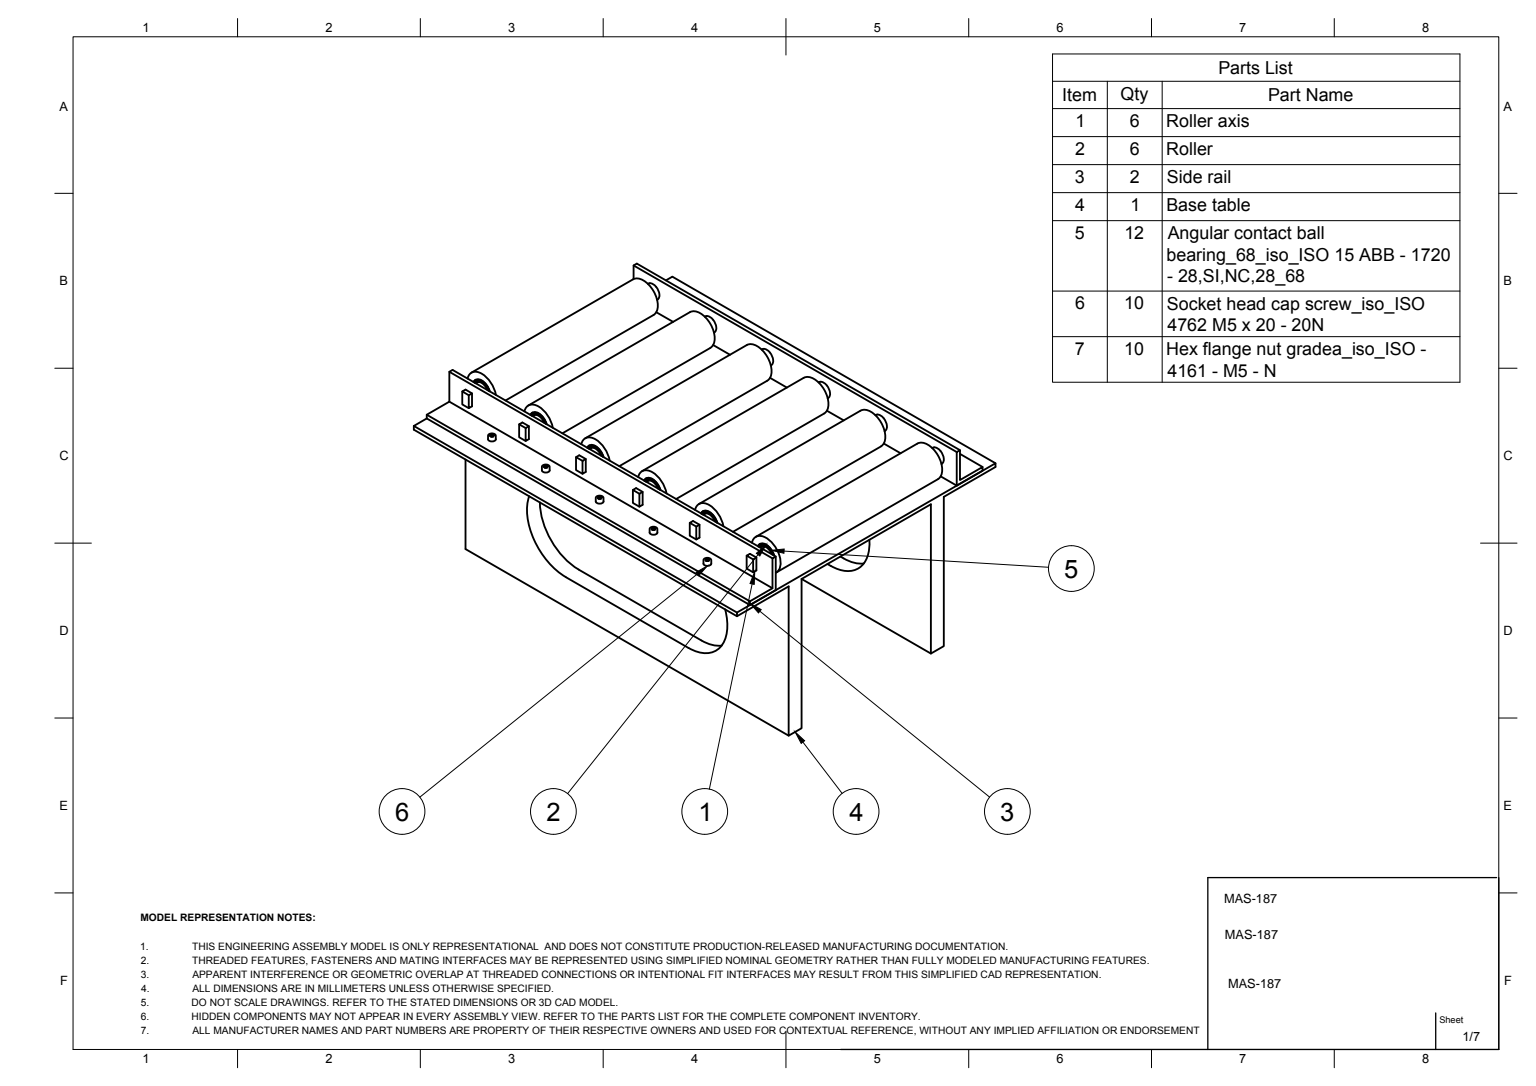
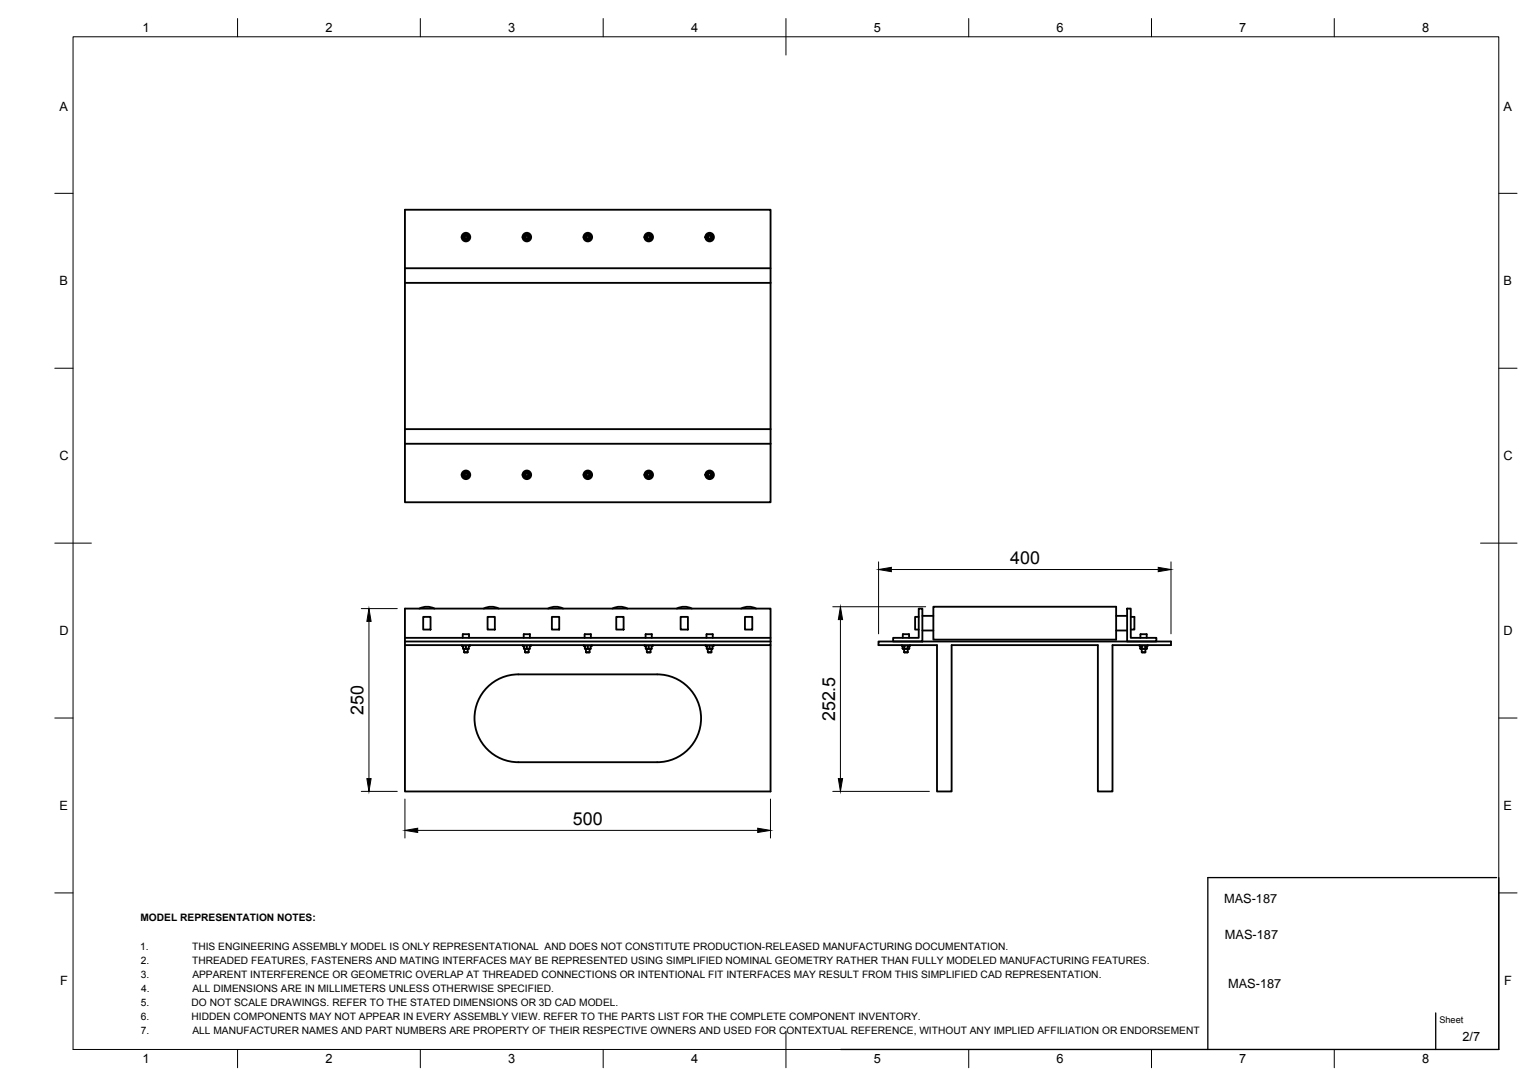
ISO-10303-21;
HEADER;
/* Generated by software containing ST-Developer
 * from STEP Tools, Inc. (www.steptools.com) 
 */

FILE_DESCRIPTION(
/* description */ ('STEP AP214'),
/* implementation_level */ '2;1');

FILE_NAME(
/* name */ 'MAS-187',
/* time_stamp */ '2026-11-04T19:00:26-08:00',
/* author */ (''),
/* organization */ (''),
/* preprocessor_version */ 'ST-DEVELOPER v20.2',
/* originating_system */ 'Autodesk Translation Framework v15.17.0.0',
/* authorisation */ '');

FILE_SCHEMA (('AUTOMOTIVE_DESIGN { 1 0 10303 214 3 1 1 }'));
ENDSEC;

DATA;
#10=MECHANICAL_DESIGN_GEOMETRIC_PRESENTATION_REPRESENTATION('',(#271,#272,
#273,#274,#275,#276,#277),#5689);
#11=ITEM_DEFINED_TRANSFORMATION($,$,#3156,#3322);
#12=ITEM_DEFINED_TRANSFORMATION($,$,#3229,#3323);
#13=ITEM_DEFINED_TRANSFORMATION($,$,#3108,#3324);
#14=ITEM_DEFINED_TRANSFORMATION($,$,#3047,#3325);
#15=ITEM_DEFINED_TRANSFORMATION($,$,#3186,#3326);
#16=ITEM_DEFINED_TRANSFORMATION($,$,#3246,#3327);
#17=ITEM_DEFINED_TRANSFORMATION($,$,#3284,#3328);
#18=ITEM_DEFINED_TRANSFORMATION($,$,#3186,#3329);
#19=ITEM_DEFINED_TRANSFORMATION($,$,#3246,#3330);
#20=ITEM_DEFINED_TRANSFORMATION($,$,#3246,#3331);
#21=ITEM_DEFINED_TRANSFORMATION($,$,#3246,#3332);
#22=ITEM_DEFINED_TRANSFORMATION($,$,#3246,#3333);
#23=ITEM_DEFINED_TRANSFORMATION($,$,#3284,#3334);
#24=ITEM_DEFINED_TRANSFORMATION($,$,#3284,#3335);
#25=ITEM_DEFINED_TRANSFORMATION($,$,#3284,#3336);
#26=ITEM_DEFINED_TRANSFORMATION($,$,#3284,#3337);
#27=ITEM_DEFINED_TRANSFORMATION($,$,#3108,#3338);
#28=ITEM_DEFINED_TRANSFORMATION($,$,#3186,#3339);
#29=ITEM_DEFINED_TRANSFORMATION($,$,#3186,#3340);
#30=ITEM_DEFINED_TRANSFORMATION($,$,#3186,#3341);
#31=ITEM_DEFINED_TRANSFORMATION($,$,#3186,#3342);
#32=ITEM_DEFINED_TRANSFORMATION($,$,#3186,#3343);
#33=ITEM_DEFINED_TRANSFORMATION($,$,#3156,#3344);
#34=ITEM_DEFINED_TRANSFORMATION($,$,#3156,#3345);
#35=ITEM_DEFINED_TRANSFORMATION($,$,#3156,#3346);
#36=ITEM_DEFINED_TRANSFORMATION($,$,#3156,#3347);
#37=ITEM_DEFINED_TRANSFORMATION($,$,#3156,#3348);
#38=ITEM_DEFINED_TRANSFORMATION($,$,#3186,#3349);
#39=ITEM_DEFINED_TRANSFORMATION($,$,#3186,#3350);
#40=ITEM_DEFINED_TRANSFORMATION($,$,#3186,#3351);
#41=ITEM_DEFINED_TRANSFORMATION($,$,#3186,#3352);
#42=ITEM_DEFINED_TRANSFORMATION($,$,#3186,#3353);
#43=ITEM_DEFINED_TRANSFORMATION($,$,#3229,#3354);
#44=ITEM_DEFINED_TRANSFORMATION($,$,#3229,#3355);
#45=ITEM_DEFINED_TRANSFORMATION($,$,#3229,#3356);
#46=ITEM_DEFINED_TRANSFORMATION($,$,#3229,#3357);
#47=ITEM_DEFINED_TRANSFORMATION($,$,#3229,#3358);
#48=ITEM_DEFINED_TRANSFORMATION($,$,#3284,#3359);
#49=ITEM_DEFINED_TRANSFORMATION($,$,#3284,#3360);
#50=ITEM_DEFINED_TRANSFORMATION($,$,#3246,#3361);
#51=ITEM_DEFINED_TRANSFORMATION($,$,#3284,#3362);
#52=ITEM_DEFINED_TRANSFORMATION($,$,#3246,#3363);
#53=ITEM_DEFINED_TRANSFORMATION($,$,#3246,#3364);
#54=ITEM_DEFINED_TRANSFORMATION($,$,#3246,#3365);
#55=ITEM_DEFINED_TRANSFORMATION($,$,#3246,#3366);
#56=ITEM_DEFINED_TRANSFORMATION($,$,#3284,#3367);
#57=ITEM_DEFINED_TRANSFORMATION($,$,#3284,#3368);
#58=(
REPRESENTATION_RELATIONSHIP($,$,#5760,#5757)
REPRESENTATION_RELATIONSHIP_WITH_TRANSFORMATION(#11)
SHAPE_REPRESENTATION_RELATIONSHIP()
);
#59=(
REPRESENTATION_RELATIONSHIP($,$,#5762,#5757)
REPRESENTATION_RELATIONSHIP_WITH_TRANSFORMATION(#12)
SHAPE_REPRESENTATION_RELATIONSHIP()
);
#60=(
REPRESENTATION_RELATIONSHIP($,$,#5759,#5757)
REPRESENTATION_RELATIONSHIP_WITH_TRANSFORMATION(#13)
SHAPE_REPRESENTATION_RELATIONSHIP()
);
#61=(
REPRESENTATION_RELATIONSHIP($,$,#5758,#5757)
REPRESENTATION_RELATIONSHIP_WITH_TRANSFORMATION(#14)
SHAPE_REPRESENTATION_RELATIONSHIP()
);
#62=(
REPRESENTATION_RELATIONSHIP($,$,#5761,#5757)
REPRESENTATION_RELATIONSHIP_WITH_TRANSFORMATION(#15)
SHAPE_REPRESENTATION_RELATIONSHIP()
);
#63=(
REPRESENTATION_RELATIONSHIP($,$,#5763,#5757)
REPRESENTATION_RELATIONSHIP_WITH_TRANSFORMATION(#16)
SHAPE_REPRESENTATION_RELATIONSHIP()
);
#64=(
REPRESENTATION_RELATIONSHIP($,$,#5764,#5757)
REPRESENTATION_RELATIONSHIP_WITH_TRANSFORMATION(#17)
SHAPE_REPRESENTATION_RELATIONSHIP()
);
#65=(
REPRESENTATION_RELATIONSHIP($,$,#5761,#5757)
REPRESENTATION_RELATIONSHIP_WITH_TRANSFORMATION(#18)
SHAPE_REPRESENTATION_RELATIONSHIP()
);
#66=(
REPRESENTATION_RELATIONSHIP($,$,#5763,#5757)
REPRESENTATION_RELATIONSHIP_WITH_TRANSFORMATION(#19)
SHAPE_REPRESENTATION_RELATIONSHIP()
);
#67=(
REPRESENTATION_RELATIONSHIP($,$,#5763,#5757)
REPRESENTATION_RELATIONSHIP_WITH_TRANSFORMATION(#20)
SHAPE_REPRESENTATION_RELATIONSHIP()
);
#68=(
REPRESENTATION_RELATIONSHIP($,$,#5763,#5757)
REPRESENTATION_RELATIONSHIP_WITH_TRANSFORMATION(#21)
SHAPE_REPRESENTATION_RELATIONSHIP()
);
#69=(
REPRESENTATION_RELATIONSHIP($,$,#5763,#5757)
REPRESENTATION_RELATIONSHIP_WITH_TRANSFORMATION(#22)
SHAPE_REPRESENTATION_RELATIONSHIP()
);
#70=(
REPRESENTATION_RELATIONSHIP($,$,#5764,#5757)
REPRESENTATION_RELATIONSHIP_WITH_TRANSFORMATION(#23)
SHAPE_REPRESENTATION_RELATIONSHIP()
);
#71=(
REPRESENTATION_RELATIONSHIP($,$,#5764,#5757)
REPRESENTATION_RELATIONSHIP_WITH_TRANSFORMATION(#24)
SHAPE_REPRESENTATION_RELATIONSHIP()
);
#72=(
REPRESENTATION_RELATIONSHIP($,$,#5764,#5757)
REPRESENTATION_RELATIONSHIP_WITH_TRANSFORMATION(#25)
SHAPE_REPRESENTATION_RELATIONSHIP()
);
#73=(
REPRESENTATION_RELATIONSHIP($,$,#5764,#5757)
REPRESENTATION_RELATIONSHIP_WITH_TRANSFORMATION(#26)
SHAPE_REPRESENTATION_RELATIONSHIP()
);
#74=(
REPRESENTATION_RELATIONSHIP($,$,#5759,#5757)
REPRESENTATION_RELATIONSHIP_WITH_TRANSFORMATION(#27)
SHAPE_REPRESENTATION_RELATIONSHIP()
);
#75=(
REPRESENTATION_RELATIONSHIP($,$,#5761,#5757)
REPRESENTATION_RELATIONSHIP_WITH_TRANSFORMATION(#28)
SHAPE_REPRESENTATION_RELATIONSHIP()
);
#76=(
REPRESENTATION_RELATIONSHIP($,$,#5761,#5757)
REPRESENTATION_RELATIONSHIP_WITH_TRANSFORMATION(#29)
SHAPE_REPRESENTATION_RELATIONSHIP()
);
#77=(
REPRESENTATION_RELATIONSHIP($,$,#5761,#5757)
REPRESENTATION_RELATIONSHIP_WITH_TRANSFORMATION(#30)
SHAPE_REPRESENTATION_RELATIONSHIP()
);
#78=(
REPRESENTATION_RELATIONSHIP($,$,#5761,#5757)
REPRESENTATION_RELATIONSHIP_WITH_TRANSFORMATION(#31)
SHAPE_REPRESENTATION_RELATIONSHIP()
);
#79=(
REPRESENTATION_RELATIONSHIP($,$,#5761,#5757)
REPRESENTATION_RELATIONSHIP_WITH_TRANSFORMATION(#32)
SHAPE_REPRESENTATION_RELATIONSHIP()
);
#80=(
REPRESENTATION_RELATIONSHIP($,$,#5760,#5757)
REPRESENTATION_RELATIONSHIP_WITH_TRANSFORMATION(#33)
SHAPE_REPRESENTATION_RELATIONSHIP()
);
#81=(
REPRESENTATION_RELATIONSHIP($,$,#5760,#5757)
REPRESENTATION_RELATIONSHIP_WITH_TRANSFORMATION(#34)
SHAPE_REPRESENTATION_RELATIONSHIP()
);
#82=(
REPRESENTATION_RELATIONSHIP($,$,#5760,#5757)
REPRESENTATION_RELATIONSHIP_WITH_TRANSFORMATION(#35)
SHAPE_REPRESENTATION_RELATIONSHIP()
);
#83=(
REPRESENTATION_RELATIONSHIP($,$,#5760,#5757)
REPRESENTATION_RELATIONSHIP_WITH_TRANSFORMATION(#36)
SHAPE_REPRESENTATION_RELATIONSHIP()
);
#84=(
REPRESENTATION_RELATIONSHIP($,$,#5760,#5757)
REPRESENTATION_RELATIONSHIP_WITH_TRANSFORMATION(#37)
SHAPE_REPRESENTATION_RELATIONSHIP()
);
#85=(
REPRESENTATION_RELATIONSHIP($,$,#5761,#5757)
REPRESENTATION_RELATIONSHIP_WITH_TRANSFORMATION(#38)
SHAPE_REPRESENTATION_RELATIONSHIP()
);
#86=(
REPRESENTATION_RELATIONSHIP($,$,#5761,#5757)
REPRESENTATION_RELATIONSHIP_WITH_TRANSFORMATION(#39)
SHAPE_REPRESENTATION_RELATIONSHIP()
);
#87=(
REPRESENTATION_RELATIONSHIP($,$,#5761,#5757)
REPRESENTATION_RELATIONSHIP_WITH_TRANSFORMATION(#40)
SHAPE_REPRESENTATION_RELATIONSHIP()
);
#88=(
REPRESENTATION_RELATIONSHIP($,$,#5761,#5757)
REPRESENTATION_RELATIONSHIP_WITH_TRANSFORMATION(#41)
SHAPE_REPRESENTATION_RELATIONSHIP()
);
#89=(
REPRESENTATION_RELATIONSHIP($,$,#5761,#5757)
REPRESENTATION_RELATIONSHIP_WITH_TRANSFORMATION(#42)
SHAPE_REPRESENTATION_RELATIONSHIP()
);
#90=(
REPRESENTATION_RELATIONSHIP($,$,#5762,#5757)
REPRESENTATION_RELATIONSHIP_WITH_TRANSFORMATION(#43)
SHAPE_REPRESENTATION_RELATIONSHIP()
);
#91=(
REPRESENTATION_RELATIONSHIP($,$,#5762,#5757)
REPRESENTATION_RELATIONSHIP_WITH_TRANSFORMATION(#44)
SHAPE_REPRESENTATION_RELATIONSHIP()
);
#92=(
REPRESENTATION_RELATIONSHIP($,$,#5762,#5757)
REPRESENTATION_RELATIONSHIP_WITH_TRANSFORMATION(#45)
SHAPE_REPRESENTATION_RELATIONSHIP()
);
#93=(
REPRESENTATION_RELATIONSHIP($,$,#5762,#5757)
REPRESENTATION_RELATIONSHIP_WITH_TRANSFORMATION(#46)
SHAPE_REPRESENTATION_RELATIONSHIP()
);
#94=(
REPRESENTATION_RELATIONSHIP($,$,#5762,#5757)
REPRESENTATION_RELATIONSHIP_WITH_TRANSFORMATION(#47)
SHAPE_REPRESENTATION_RELATIONSHIP()
);
#95=(
REPRESENTATION_RELATIONSHIP($,$,#5764,#5757)
REPRESENTATION_RELATIONSHIP_WITH_TRANSFORMATION(#48)
SHAPE_REPRESENTATION_RELATIONSHIP()
);
#96=(
REPRESENTATION_RELATIONSHIP($,$,#5764,#5757)
REPRESENTATION_RELATIONSHIP_WITH_TRANSFORMATION(#49)
SHAPE_REPRESENTATION_RELATIONSHIP()
);
#97=(
REPRESENTATION_RELATIONSHIP($,$,#5763,#5757)
REPRESENTATION_RELATIONSHIP_WITH_TRANSFORMATION(#50)
SHAPE_REPRESENTATION_RELATIONSHIP()
);
#98=(
REPRESENTATION_RELATIONSHIP($,$,#5764,#5757)
REPRESENTATION_RELATIONSHIP_WITH_TRANSFORMATION(#51)
SHAPE_REPRESENTATION_RELATIONSHIP()
);
#99=(
REPRESENTATION_RELATIONSHIP($,$,#5763,#5757)
REPRESENTATION_RELATIONSHIP_WITH_TRANSFORMATION(#52)
SHAPE_REPRESENTATION_RELATIONSHIP()
);
#100=(
REPRESENTATION_RELATIONSHIP($,$,#5763,#5757)
REPRESENTATION_RELATIONSHIP_WITH_TRANSFORMATION(#53)
SHAPE_REPRESENTATION_RELATIONSHIP()
);
#101=(
REPRESENTATION_RELATIONSHIP($,$,#5763,#5757)
REPRESENTATION_RELATIONSHIP_WITH_TRANSFORMATION(#54)
SHAPE_REPRESENTATION_RELATIONSHIP()
);
#102=(
REPRESENTATION_RELATIONSHIP($,$,#5763,#5757)
REPRESENTATION_RELATIONSHIP_WITH_TRANSFORMATION(#55)
SHAPE_REPRESENTATION_RELATIONSHIP()
);
#103=(
REPRESENTATION_RELATIONSHIP($,$,#5764,#5757)
REPRESENTATION_RELATIONSHIP_WITH_TRANSFORMATION(#56)
SHAPE_REPRESENTATION_RELATIONSHIP()
);
#104=(
REPRESENTATION_RELATIONSHIP($,$,#5764,#5757)
REPRESENTATION_RELATIONSHIP_WITH_TRANSFORMATION(#57)
SHAPE_REPRESENTATION_RELATIONSHIP()
);
#105=CONTEXT_DEPENDENT_SHAPE_REPRESENTATION(#58,#5710);
#106=CONTEXT_DEPENDENT_SHAPE_REPRESENTATION(#59,#5711);
#107=CONTEXT_DEPENDENT_SHAPE_REPRESENTATION(#60,#5712);
#108=CONTEXT_DEPENDENT_SHAPE_REPRESENTATION(#61,#5713);
#109=CONTEXT_DEPENDENT_SHAPE_REPRESENTATION(#62,#5714);
#110=CONTEXT_DEPENDENT_SHAPE_REPRESENTATION(#63,#5715);
#111=CONTEXT_DEPENDENT_SHAPE_REPRESENTATION(#64,#5716);
#112=CONTEXT_DEPENDENT_SHAPE_REPRESENTATION(#65,#5717);
#113=CONTEXT_DEPENDENT_SHAPE_REPRESENTATION(#66,#5718);
#114=CONTEXT_DEPENDENT_SHAPE_REPRESENTATION(#67,#5719);
#115=CONTEXT_DEPENDENT_SHAPE_REPRESENTATION(#68,#5720);
#116=CONTEXT_DEPENDENT_SHAPE_REPRESENTATION(#69,#5721);
#117=CONTEXT_DEPENDENT_SHAPE_REPRESENTATION(#70,#5722);
#118=CONTEXT_DEPENDENT_SHAPE_REPRESENTATION(#71,#5723);
#119=CONTEXT_DEPENDENT_SHAPE_REPRESENTATION(#72,#5724);
#120=CONTEXT_DEPENDENT_SHAPE_REPRESENTATION(#73,#5725);
#121=CONTEXT_DEPENDENT_SHAPE_REPRESENTATION(#74,#5726);
#122=CONTEXT_DEPENDENT_SHAPE_REPRESENTATION(#75,#5727);
#123=CONTEXT_DEPENDENT_SHAPE_REPRESENTATION(#76,#5728);
#124=CONTEXT_DEPENDENT_SHAPE_REPRESENTATION(#77,#5729);
#125=CONTEXT_DEPENDENT_SHAPE_REPRESENTATION(#78,#5730);
#126=CONTEXT_DEPENDENT_SHAPE_REPRESENTATION(#79,#5731);
#127=CONTEXT_DEPENDENT_SHAPE_REPRESENTATION(#80,#5732);
#128=CONTEXT_DEPENDENT_SHAPE_REPRESENTATION(#81,#5733);
#129=CONTEXT_DEPENDENT_SHAPE_REPRESENTATION(#82,#5734);
#130=CONTEXT_DEPENDENT_SHAPE_REPRESENTATION(#83,#5735);
#131=CONTEXT_DEPENDENT_SHAPE_REPRESENTATION(#84,#5736);
#132=CONTEXT_DEPENDENT_SHAPE_REPRESENTATION(#85,#5737);
#133=CONTEXT_DEPENDENT_SHAPE_REPRESENTATION(#86,#5738);
#134=CONTEXT_DEPENDENT_SHAPE_REPRESENTATION(#87,#5739);
#135=CONTEXT_DEPENDENT_SHAPE_REPRESENTATION(#88,#5740);
#136=CONTEXT_DEPENDENT_SHAPE_REPRESENTATION(#89,#5741);
#137=CONTEXT_DEPENDENT_SHAPE_REPRESENTATION(#90,#5742);
#138=CONTEXT_DEPENDENT_SHAPE_REPRESENTATION(#91,#5743);
#139=CONTEXT_DEPENDENT_SHAPE_REPRESENTATION(#92,#5744);
#140=CONTEXT_DEPENDENT_SHAPE_REPRESENTATION(#93,#5745);
#141=CONTEXT_DEPENDENT_SHAPE_REPRESENTATION(#94,#5746);
#142=CONTEXT_DEPENDENT_SHAPE_REPRESENTATION(#95,#5747);
#143=CONTEXT_DEPENDENT_SHAPE_REPRESENTATION(#96,#5748);
#144=CONTEXT_DEPENDENT_SHAPE_REPRESENTATION(#97,#5749);
#145=CONTEXT_DEPENDENT_SHAPE_REPRESENTATION(#98,#5750);
#146=CONTEXT_DEPENDENT_SHAPE_REPRESENTATION(#99,#5751);
#147=CONTEXT_DEPENDENT_SHAPE_REPRESENTATION(#100,#5752);
#148=CONTEXT_DEPENDENT_SHAPE_REPRESENTATION(#101,#5753);
#149=CONTEXT_DEPENDENT_SHAPE_REPRESENTATION(#102,#5754);
#150=CONTEXT_DEPENDENT_SHAPE_REPRESENTATION(#103,#5755);
#151=CONTEXT_DEPENDENT_SHAPE_REPRESENTATION(#104,#5756);
#152=NEXT_ASSEMBLY_USAGE_OCCURRENCE('roller axis:1','roller axis:1',
'roller axis:1',#5766,#5769,'roller axis:1');
#153=NEXT_ASSEMBLY_USAGE_OCCURRENCE('roller:1','roller:1','roller:1',#5766,
#5771,'roller:1');
#154=NEXT_ASSEMBLY_USAGE_OCCURRENCE('side rail:1','side rail:1',
'side rail:1',#5766,#5768,'side rail:1');
#155=NEXT_ASSEMBLY_USAGE_OCCURRENCE('base table:1','base table:1',
'base table:1',#5766,#5767,'base table:1');
#156=NEXT_ASSEMBLY_USAGE_OCCURRENCE(
'angular contact ball bearing_68_iso_ISO 15 ABB - 1720 - 28,SI,NC,28_6
8:1',
'angular contact ball bearing_68_iso_ISO 15 ABB - 1720 - 28,SI,NC,28_6
8:1',
'angular contact ball bearing_68_iso_ISO 15 ABB - 1720 - 28,SI,NC,28_6
8:1',#5766,#5770,
'angular contact ball bearing_68_iso_ISO 15 ABB - 1720 - 28,SI,NC,28_6
8:1');
#157=NEXT_ASSEMBLY_USAGE_OCCURRENCE(
'socket head cap screw_iso_ISO 4762 M5 x 20 - 20N:1',
'socket head cap screw_iso_ISO 4762 M5 x 20 - 20N:1',
'socket head cap screw_iso_ISO 4762 M5 x 20 - 20N:1',#5766,#5772,
'socket head cap screw_iso_ISO 4762 M5 x 20 - 20N:1');
#158=NEXT_ASSEMBLY_USAGE_OCCURRENCE(
'hex flange nut gradea_iso_ISO - 4161 - M5 - N:1',
'hex flange nut gradea_iso_ISO - 4161 - M5 - N:1',
'hex flange nut gradea_iso_ISO - 4161 - M5 - N:1',#5766,#5773,
'hex flange nut gradea_iso_ISO - 4161 - M5 - N:1');
#159=NEXT_ASSEMBLY_USAGE_OCCURRENCE(
'angular contact ball bearing_68_iso_ISO 15 ABB - 1720 - 28,SI,NC,28_6
8:2',
'angular contact ball bearing_68_iso_ISO 15 ABB - 1720 - 28,SI,NC,28_6
8:2',
'angular contact ball bearing_68_iso_ISO 15 ABB - 1720 - 28,SI,NC,28_6
8:2',#5766,#5770,
'angular contact ball bearing_68_iso_ISO 15 ABB - 1720 - 28,SI,NC,28_6
8:2');
#160=NEXT_ASSEMBLY_USAGE_OCCURRENCE(
'socket head cap screw_iso_ISO 4762 M5 x 20 - 20N:2',
'socket head cap screw_iso_ISO 4762 M5 x 20 - 20N:2',
'socket head cap screw_iso_ISO 4762 M5 x 20 - 20N:2',#5766,#5772,
'socket head cap screw_iso_ISO 4762 M5 x 20 - 20N:2');
#161=NEXT_ASSEMBLY_USAGE_OCCURRENCE(
'socket head cap screw_iso_ISO 4762 M5 x 20 - 20N:3',
'socket head cap screw_iso_ISO 4762 M5 x 20 - 20N:3',
'socket head cap screw_iso_ISO 4762 M5 x 20 - 20N:3',#5766,#5772,
'socket head cap screw_iso_ISO 4762 M5 x 20 - 20N:3');
#162=NEXT_ASSEMBLY_USAGE_OCCURRENCE(
'socket head cap screw_iso_ISO 4762 M5 x 20 - 20N:4',
'socket head cap screw_iso_ISO 4762 M5 x 20 - 20N:4',
'socket head cap screw_iso_ISO 4762 M5 x 20 - 20N:4',#5766,#5772,
'socket head cap screw_iso_ISO 4762 M5 x 20 - 20N:4');
#163=NEXT_ASSEMBLY_USAGE_OCCURRENCE(
'socket head cap screw_iso_ISO 4762 M5 x 20 - 20N:5',
'socket head cap screw_iso_ISO 4762 M5 x 20 - 20N:5',
'socket head cap screw_iso_ISO 4762 M5 x 20 - 20N:5',#5766,#5772,
'socket head cap screw_iso_ISO 4762 M5 x 20 - 20N:5');
#164=NEXT_ASSEMBLY_USAGE_OCCURRENCE(
'hex flange nut gradea_iso_ISO - 4161 - M5 - N:2',
'hex flange nut gradea_iso_ISO - 4161 - M5 - N:2',
'hex flange nut gradea_iso_ISO - 4161 - M5 - N:2',#5766,#5773,
'hex flange nut gradea_iso_ISO - 4161 - M5 - N:2');
#165=NEXT_ASSEMBLY_USAGE_OCCURRENCE(
'hex flange nut gradea_iso_ISO - 4161 - M5 - N:3',
'hex flange nut gradea_iso_ISO - 4161 - M5 - N:3',
'hex flange nut gradea_iso_ISO - 4161 - M5 - N:3',#5766,#5773,
'hex flange nut gradea_iso_ISO - 4161 - M5 - N:3');
#166=NEXT_ASSEMBLY_USAGE_OCCURRENCE(
'hex flange nut gradea_iso_ISO - 4161 - M5 - N:4',
'hex flange nut gradea_iso_ISO - 4161 - M5 - N:4',
'hex flange nut gradea_iso_ISO - 4161 - M5 - N:4',#5766,#5773,
'hex flange nut gradea_iso_ISO - 4161 - M5 - N:4');
#167=NEXT_ASSEMBLY_USAGE_OCCURRENCE(
'hex flange nut gradea_iso_ISO - 4161 - M5 - N:5',
'hex flange nut gradea_iso_ISO - 4161 - M5 - N:5',
'hex flange nut gradea_iso_ISO - 4161 - M5 - N:5',#5766,#5773,
'hex flange nut gradea_iso_ISO - 4161 - M5 - N:5');
#168=NEXT_ASSEMBLY_USAGE_OCCURRENCE('side rail:2','side rail:2',
'side rail:2',#5766,#5768,'side rail:2');
#169=NEXT_ASSEMBLY_USAGE_OCCURRENCE(
'angular contact ball bearing_68_iso_ISO 15 ABB - 1720 - 28,SI,NC,28_6
8:3',
'angular contact ball bearing_68_iso_ISO 15 ABB - 1720 - 28,SI,NC,28_6
8:3',
'angular contact ball bearing_68_iso_ISO 15 ABB - 1720 - 28,SI,NC,28_6
8:3',#5766,#5770,
'angular contact ball bearing_68_iso_ISO 15 ABB - 1720 - 28,SI,NC,28_6
8:3');
#170=NEXT_ASSEMBLY_USAGE_OCCURRENCE(
'angular contact ball bearing_68_iso_ISO 15 ABB - 1720 - 28,SI,NC,28_6
8:4',
'angular contact ball bearing_68_iso_ISO 15 ABB - 1720 - 28,SI,NC,28_6
8:4',
'angular contact ball bearing_68_iso_ISO 15 ABB - 1720 - 28,SI,NC,28_6
8:4',#5766,#5770,
'angular contact ball bearing_68_iso_ISO 15 ABB - 1720 - 28,SI,NC,28_6
8:4');
#171=NEXT_ASSEMBLY_USAGE_OCCURRENCE(
'angular contact ball bearing_68_iso_ISO 15 ABB - 1720 - 28,SI,NC,28_6
8:5',
'angular contact ball bearing_68_iso_ISO 15 ABB - 1720 - 28,SI,NC,28_6
8:5',
'angular contact ball bearing_68_iso_ISO 15 ABB - 1720 - 28,SI,NC,28_6
8:5',#5766,#5770,
'angular contact ball bearing_68_iso_ISO 15 ABB - 1720 - 28,SI,NC,28_6
8:5');
#172=NEXT_ASSEMBLY_USAGE_OCCURRENCE(
'angular contact ball bearing_68_iso_ISO 15 ABB - 1720 - 28,SI,NC,28_6
8:6',
'angular contact ball bearing_68_iso_ISO 15 ABB - 1720 - 28,SI,NC,28_6
8:6',
'angular contact ball bearing_68_iso_ISO 15 ABB - 1720 - 28,SI,NC,28_6
8:6',#5766,#5770,
'angular contact ball bearing_68_iso_ISO 15 ABB - 1720 - 28,SI,NC,28_6
8:6');
#173=NEXT_ASSEMBLY_USAGE_OCCURRENCE(
'angular contact ball bearing_68_iso_ISO 15 ABB - 1720 - 28,SI,NC,28_6
8:7',
'angular contact ball bearing_68_iso_ISO 15 ABB - 1720 - 28,SI,NC,28_6
8:7',
'angular contact ball bearing_68_iso_ISO 15 ABB - 1720 - 28,SI,NC,28_6
8:7',#5766,#5770,
'angular contact ball bearing_68_iso_ISO 15 ABB - 1720 - 28,SI,NC,28_6
8:7');
#174=NEXT_ASSEMBLY_USAGE_OCCURRENCE('roller axis:2','roller axis:2',
'roller axis:2',#5766,#5769,'roller axis:2');
#175=NEXT_ASSEMBLY_USAGE_OCCURRENCE('roller axis:3','roller axis:3',
'roller axis:3',#5766,#5769,'roller axis:3');
#176=NEXT_ASSEMBLY_USAGE_OCCURRENCE('roller axis:4','roller axis:4',
'roller axis:4',#5766,#5769,'roller axis:4');
#177=NEXT_ASSEMBLY_USAGE_OCCURRENCE('roller axis:5','roller axis:5',
'roller axis:5',#5766,#5769,'roller axis:5');
#178=NEXT_ASSEMBLY_USAGE_OCCURRENCE('roller axis:6','roller axis:6',
'roller axis:6',#5766,#5769,'roller axis:6');
#179=NEXT_ASSEMBLY_USAGE_OCCURRENCE(
'angular contact ball bearing_68_iso_ISO 15 ABB - 1720 - 28,SI,NC,28_6
8:8',
'angular contact ball bearing_68_iso_ISO 15 ABB - 1720 - 28,SI,NC,28_6
8:8',
'angular contact ball bearing_68_iso_ISO 15 ABB - 1720 - 28,SI,NC,28_6
8:8',#5766,#5770,
'angular contact ball bearing_68_iso_ISO 15 ABB - 1720 - 28,SI,NC,28_6
8:8');
#180=NEXT_ASSEMBLY_USAGE_OCCURRENCE(
'angular contact ball bearing_68_iso_ISO 15 ABB - 1720 - 28,SI,NC,28_6
8:9',
'angular contact ball bearing_68_iso_ISO 15 ABB - 1720 - 28,SI,NC,28_6
8:9',
'angular contact ball bearing_68_iso_ISO 15 ABB - 1720 - 28,SI,NC,28_6
8:9',#5766,#5770,
'angular contact ball bearing_68_iso_ISO 15 ABB - 1720 - 28,SI,NC,28_6
8:9');
#181=NEXT_ASSEMBLY_USAGE_OCCURRENCE(
'angular contact ball bearing_68_iso_ISO 15 ABB - 1720 - 28,SI,NC,28_6
8:10',
'angular contact ball bearing_68_iso_ISO 15 ABB - 1720 - 28,SI,NC,28_6
8:10',
'angular contact ball bearing_68_iso_ISO 15 ABB - 1720 - 28,SI,NC,28_6
8:10',#5766,#5770,
'angular contact ball bearing_68_iso_ISO 15 ABB - 1720 - 28,SI,NC,28_6
8:10');
#182=NEXT_ASSEMBLY_USAGE_OCCURRENCE(
'angular contact ball bearing_68_iso_ISO 15 ABB - 1720 - 28,SI,NC,28_6
8:11',
'angular contact ball bearing_68_iso_ISO 15 ABB - 1720 - 28,SI,NC,28_6
8:11',
'angular contact ball bearing_68_iso_ISO 15 ABB - 1720 - 28,SI,NC,28_6
8:11',#5766,#5770,
'angular contact ball bearing_68_iso_ISO 15 ABB - 1720 - 28,SI,NC,28_6
8:11');
#183=NEXT_ASSEMBLY_USAGE_OCCURRENCE(
'angular contact ball bearing_68_iso_ISO 15 ABB - 1720 - 28,SI,NC,28_6
8:12',
'angular contact ball bearing_68_iso_ISO 15 ABB - 1720 - 28,SI,NC,28_6
8:12',
'angular contact ball bearing_68_iso_ISO 15 ABB - 1720 - 28,SI,NC,28_6
8:12',#5766,#5770,
'angular contact ball bearing_68_iso_ISO 15 ABB - 1720 - 28,SI,NC,28_6
8:12');
#184=NEXT_ASSEMBLY_USAGE_OCCURRENCE('roller:2','roller:2','roller:2',#5766,
#5771,'roller:2');
#185=NEXT_ASSEMBLY_USAGE_OCCURRENCE('roller:3','roller:3','roller:3',#5766,
#5771,'roller:3');
#186=NEXT_ASSEMBLY_USAGE_OCCURRENCE('roller:4','roller:4','roller:4',#5766,
#5771,'roller:4');
#187=NEXT_ASSEMBLY_USAGE_OCCURRENCE('roller:5','roller:5','roller:5',#5766,
#5771,'roller:5');
#188=NEXT_ASSEMBLY_USAGE_OCCURRENCE('roller:6','roller:6','roller:6',#5766,
#5771,'roller:6');
#189=NEXT_ASSEMBLY_USAGE_OCCURRENCE(
'hex flange nut gradea_iso_ISO - 4161 - M5 - N:6',
'hex flange nut gradea_iso_ISO - 4161 - M5 - N:6',
'hex flange nut gradea_iso_ISO - 4161 - M5 - N:6',#5766,#5773,
'hex flange nut gradea_iso_ISO - 4161 - M5 - N:6');
#190=NEXT_ASSEMBLY_USAGE_OCCURRENCE(
'hex flange nut gradea_iso_ISO - 4161 - M5 - N:7',
'hex flange nut gradea_iso_ISO - 4161 - M5 - N:7',
'hex flange nut gradea_iso_ISO - 4161 - M5 - N:7',#5766,#5773,
'hex flange nut gradea_iso_ISO - 4161 - M5 - N:7');
#191=NEXT_ASSEMBLY_USAGE_OCCURRENCE(
'socket head cap screw_iso_ISO 4762 M5 x 20 - 20N:6',
'socket head cap screw_iso_ISO 4762 M5 x 20 - 20N:6',
'socket head cap screw_iso_ISO 4762 M5 x 20 - 20N:6',#5766,#5772,
'socket head cap screw_iso_ISO 4762 M5 x 20 - 20N:6');
#192=NEXT_ASSEMBLY_USAGE_OCCURRENCE(
'hex flange nut gradea_iso_ISO - 4161 - M5 - N:8',
'hex flange nut gradea_iso_ISO - 4161 - M5 - N:8',
'hex flange nut gradea_iso_ISO - 4161 - M5 - N:8',#5766,#5773,
'hex flange nut gradea_iso_ISO - 4161 - M5 - N:8');
#193=NEXT_ASSEMBLY_USAGE_OCCURRENCE(
'socket head cap screw_iso_ISO 4762 M5 x 20 - 20N:7',
'socket head cap screw_iso_ISO 4762 M5 x 20 - 20N:7',
'socket head cap screw_iso_ISO 4762 M5 x 20 - 20N:7',#5766,#5772,
'socket head cap screw_iso_ISO 4762 M5 x 20 - 20N:7');
#194=NEXT_ASSEMBLY_USAGE_OCCURRENCE(
'socket head cap screw_iso_ISO 4762 M5 x 20 - 20N:8',
'socket head cap screw_iso_ISO 4762 M5 x 20 - 20N:8',
'socket head cap screw_iso_ISO 4762 M5 x 20 - 20N:8',#5766,#5772,
'socket head cap screw_iso_ISO 4762 M5 x 20 - 20N:8');
#195=NEXT_ASSEMBLY_USAGE_OCCURRENCE(
'socket head cap screw_iso_ISO 4762 M5 x 20 - 20N:9',
'socket head cap screw_iso_ISO 4762 M5 x 20 - 20N:9',
'socket head cap screw_iso_ISO 4762 M5 x 20 - 20N:9',#5766,#5772,
'socket head cap screw_iso_ISO 4762 M5 x 20 - 20N:9');
#196=NEXT_ASSEMBLY_USAGE_OCCURRENCE(
'socket head cap screw_iso_ISO 4762 M5 x 20 - 20N:10',
'socket head cap screw_iso_ISO 4762 M5 x 20 - 20N:10',
'socket head cap screw_iso_ISO 4762 M5 x 20 - 20N:10',#5766,#5772,
'socket head cap screw_iso_ISO 4762 M5 x 20 - 20N:10');
#197=NEXT_ASSEMBLY_USAGE_OCCURRENCE(
'hex flange nut gradea_iso_ISO - 4161 - M5 - N:9',
'hex flange nut gradea_iso_ISO - 4161 - M5 - N:9',
'hex flange nut gradea_iso_ISO - 4161 - M5 - N:9',#5766,#5773,
'hex flange nut gradea_iso_ISO - 4161 - M5 - N:9');
#198=NEXT_ASSEMBLY_USAGE_OCCURRENCE(
'hex flange nut gradea_iso_ISO - 4161 - M5 - N:10',
'hex flange nut gradea_iso_ISO - 4161 - M5 - N:10',
'hex flange nut gradea_iso_ISO - 4161 - M5 - N:10',#5766,#5773,
'hex flange nut gradea_iso_ISO - 4161 - M5 - N:10');
#199=(
BOUNDED_SURFACE()
B_SPLINE_SURFACE(3,2,((#5358,#5359,#5360),(#5361,#5362,#5363),(#5364,#5365,
#5366),(#5367,#5368,#5369),(#5370,#5371,#5372),(#5373,#5374,#5375)),
 .UNSPECIFIED.,.F.,.F.,.F.)
B_SPLINE_SURFACE_WITH_KNOTS((4,2,4),(3,3),(0.0203285324751813,0.0227886329536482,
0.0252487334321152),(0.,1.),.UNSPECIFIED.)
GEOMETRIC_REPRESENTATION_ITEM()
RATIONAL_B_SPLINE_SURFACE(((1.,0.804778161589684,1.),(1.,0.812376758628819,
1.),(1.,0.819066241556581,1.),(1.,0.81923610156676,1.),(1.,0.812613580710497,
1.),(1.,0.804771233831858,1.)))
REPRESENTATION_ITEM('')
SURFACE()
);
#200=(
BOUNDED_SURFACE()
B_SPLINE_SURFACE(3,2,((#5429,#5430,#5431),(#5432,#5433,#5434),(#5435,#5436,
#5437),(#5438,#5439,#5440),(#5441,#5442,#5443),(#5444,#5445,#5446)),
 .UNSPECIFIED.,.F.,.F.,.F.)
B_SPLINE_SURFACE_WITH_KNOTS((4,2,4),(3,3),(0.0203285324751813,0.0227886329536482,
0.0252487334321152),(0.,1.),.UNSPECIFIED.)
GEOMETRIC_REPRESENTATION_ITEM()
RATIONAL_B_SPLINE_SURFACE(((1.,0.804778161589684,1.),(1.,0.812376758628925,
1.),(1.,0.819066241556439,1.),(1.,0.819236101566903,1.),(1.,0.81261358071039,
1.),(1.,0.804771233831859,1.)))
REPRESENTATION_ITEM('')
SURFACE()
);
#201=(
BOUNDED_SURFACE()
B_SPLINE_SURFACE(3,2,((#5472,#5473,#5474),(#5475,#5476,#5477),(#5478,#5479,
#5480),(#5481,#5482,#5483),(#5484,#5485,#5486),(#5487,#5488,#5489)),
 .UNSPECIFIED.,.F.,.F.,.F.)
B_SPLINE_SURFACE_WITH_KNOTS((4,2,4),(3,3),(0.0202775271026916,0.022737815950911,
0.0251981047991304),(0.,1.),.UNSPECIFIED.)
GEOMETRIC_REPRESENTATION_ITEM()
RATIONAL_B_SPLINE_SURFACE(((1.,0.804778143171281,1.),(1.,0.812377324708393,
1.),(1.,0.819067019215491,1.),(1.,0.819235355291218,1.),(1.,0.812613209822683,
1.),(1.,0.804771246585639,1.)))
REPRESENTATION_ITEM('')
SURFACE()
);
#202=(
BOUNDED_SURFACE()
B_SPLINE_SURFACE(3,2,((#5518,#5519,#5520),(#5521,#5522,#5523),(#5524,#5525,
#5526),(#5527,#5528,#5529),(#5530,#5531,#5532),(#5533,#5534,#5535)),
 .UNSPECIFIED.,.F.,.F.,.F.)
B_SPLINE_SURFACE_WITH_KNOTS((4,2,4),(3,3),(0.0202706586107177,0.0227307226783692,
0.0251907867460207),(0.,1.),.UNSPECIFIED.)
GEOMETRIC_REPRESENTATION_ITEM()
RATIONAL_B_SPLINE_SURFACE(((1.,0.80477817083373,1.),(1.,0.812376519070531,
1.),(1.,0.819065627716398,1.),(1.,0.819236690351216,1.),(1.,0.812613845430289,
1.),(1.,0.804771224603142,1.)))
REPRESENTATION_ITEM('')
SURFACE()
);
#203=(
BOUNDED_SURFACE()
B_SPLINE_SURFACE(3,2,((#5561,#5562,#5563),(#5564,#5565,#5566),(#5567,#5568,
#5569),(#5570,#5571,#5572),(#5573,#5574,#5575),(#5576,#5577,#5578)),
 .UNSPECIFIED.,.F.,.F.,.F.)
B_SPLINE_SURFACE_WITH_KNOTS((4,2,4),(3,3),(0.0203285324751813,0.0227886329536482,
0.0252487334321152),(0.,1.),.UNSPECIFIED.)
GEOMETRIC_REPRESENTATION_ITEM()
RATIONAL_B_SPLINE_SURFACE(((1.,0.804778161589684,1.),(1.,0.812376758628997,
1.),(1.,0.819066241556344,1.),(1.,0.819236101566998,1.),(1.,0.812613580710318,
1.),(1.,0.804771233831859,1.)))
REPRESENTATION_ITEM('')
SURFACE()
);
#204=(
BOUNDED_SURFACE()
B_SPLINE_SURFACE(3,2,((#5607,#5608,#5609),(#5610,#5611,#5612),(#5613,#5614,
#5615),(#5616,#5617,#5618),(#5619,#5620,#5621),(#5622,#5623,#5624)),
 .UNSPECIFIED.,.F.,.F.,.F.)
B_SPLINE_SURFACE_WITH_KNOTS((4,2,4),(3,3),(0.0203285324751813,0.0227886329536482,
0.0252487334321152),(0.,1.),.UNSPECIFIED.)
GEOMETRIC_REPRESENTATION_ITEM()
RATIONAL_B_SPLINE_SURFACE(((1.,0.804778161589684,1.),(1.,0.812376758629104,
1.),(1.,0.819066241556201,1.),(1.,0.81923610156714,1.),(1.,0.812613580710212,
1.),(1.,0.804771233831859,1.)))
REPRESENTATION_ITEM('')
SURFACE()
);
#205=(
BOUNDED_CURVE()
B_SPLINE_CURVE(2,(#5146,#5147,#5148),.UNSPECIFIED.,.F.,.F.)
B_SPLINE_CURVE_WITH_KNOTS((3,3),(0.56122233924649,0.967776243738921),
 .UNSPECIFIED.)
CURVE()
GEOMETRIC_REPRESENTATION_ITEM()
RATIONAL_B_SPLINE_CURVE((1.56483201089635,1.68587218817573,1.68587218817573))
REPRESENTATION_ITEM('')
);
#206=(
BOUNDED_CURVE()
B_SPLINE_CURVE(2,(#5149,#5150,#5151),.UNSPECIFIED.,.F.,.F.)
B_SPLINE_CURVE_WITH_KNOTS((3,3),(0.967776243738921,1.37433014823136),
 .UNSPECIFIED.)
CURVE()
GEOMETRIC_REPRESENTATION_ITEM()
RATIONAL_B_SPLINE_CURVE((1.68587218817573,1.68587218817573,1.56483201089635))
REPRESENTATION_ITEM('')
);
#207=(
BOUNDED_CURVE()
B_SPLINE_CURVE(2,(#5185,#5186,#5187),.UNSPECIFIED.,.F.,.F.)
B_SPLINE_CURVE_WITH_KNOTS((3,3),(0.561222339246465,0.967776243738892),
 .UNSPECIFIED.)
CURVE()
GEOMETRIC_REPRESENTATION_ITEM()
RATIONAL_B_SPLINE_CURVE((1.56483201089633,1.6858721881757,1.6858721881757))
REPRESENTATION_ITEM('')
);
#208=(
BOUNDED_CURVE()
B_SPLINE_CURVE(2,(#5188,#5189,#5190),.UNSPECIFIED.,.F.,.F.)
B_SPLINE_CURVE_WITH_KNOTS((3,3),(0.967776243738892,1.37433014823131),
 .UNSPECIFIED.)
CURVE()
GEOMETRIC_REPRESENTATION_ITEM()
RATIONAL_B_SPLINE_CURVE((1.6858721881757,1.6858721881757,1.56483201089633))
REPRESENTATION_ITEM('')
);
#209=(
BOUNDED_CURVE()
B_SPLINE_CURVE(2,(#5224,#5225,#5226),.UNSPECIFIED.,.F.,.F.)
B_SPLINE_CURVE_WITH_KNOTS((3,3),(0.967776300881118,1.37433022008006),
 .UNSPECIFIED.)
CURVE()
GEOMETRIC_REPRESENTATION_ITEM()
RATIONAL_B_SPLINE_CURVE((1.68587224106752,1.68587224106752,1.56483205999068))
REPRESENTATION_ITEM('')
);
#210=(
BOUNDED_CURVE()
B_SPLINE_CURVE(2,(#5227,#5228,#5229),.UNSPECIFIED.,.F.,.F.)
B_SPLINE_CURVE_WITH_KNOTS((3,3),(0.561222381682178,0.967776300881118),
 .UNSPECIFIED.)
CURVE()
GEOMETRIC_REPRESENTATION_ITEM()
RATIONAL_B_SPLINE_CURVE((1.56483205999068,1.68587224106752,1.68587224106752))
REPRESENTATION_ITEM('')
);
#211=(
BOUNDED_CURVE()
B_SPLINE_CURVE(2,(#5263,#5264,#5265),.UNSPECIFIED.,.F.,.F.)
B_SPLINE_CURVE_WITH_KNOTS((3,3),(0.561222339246487,0.967776243738916),
 .UNSPECIFIED.)
CURVE()
GEOMETRIC_REPRESENTATION_ITEM()
RATIONAL_B_SPLINE_CURVE((1.56483201089635,1.68587218817572,1.68587218817572))
REPRESENTATION_ITEM('')
);
#212=(
BOUNDED_CURVE()
B_SPLINE_CURVE(2,(#5266,#5267,#5268),.UNSPECIFIED.,.F.,.F.)
B_SPLINE_CURVE_WITH_KNOTS((3,3),(0.967776243738916,1.37433014823135),
 .UNSPECIFIED.)
CURVE()
GEOMETRIC_REPRESENTATION_ITEM()
RATIONAL_B_SPLINE_CURVE((1.68587218817572,1.68587218817572,1.56483201089634))
REPRESENTATION_ITEM('')
);
#213=(
BOUNDED_CURVE()
B_SPLINE_CURVE(2,(#5302,#5303,#5304),.UNSPECIFIED.,.F.,.F.)
B_SPLINE_CURVE_WITH_KNOTS((3,3),(0.561222339246469,0.967776243738892),
 .UNSPECIFIED.)
CURVE()
GEOMETRIC_REPRESENTATION_ITEM()
RATIONAL_B_SPLINE_CURVE((1.56483201089633,1.6858721881757,1.6858721881757))
REPRESENTATION_ITEM('')
);
#214=(
BOUNDED_CURVE()
B_SPLINE_CURVE(2,(#5305,#5306,#5307),.UNSPECIFIED.,.F.,.F.)
B_SPLINE_CURVE_WITH_KNOTS((3,3),(0.967776243738892,1.37433014823132),
 .UNSPECIFIED.)
CURVE()
GEOMETRIC_REPRESENTATION_ITEM()
RATIONAL_B_SPLINE_CURVE((1.6858721881757,1.6858721881757,1.56483201089633))
REPRESENTATION_ITEM('')
);
#215=(
BOUNDED_CURVE()
B_SPLINE_CURVE(2,(#5338,#5339,#5340),.UNSPECIFIED.,.F.,.F.)
B_SPLINE_CURVE_WITH_KNOTS((3,3),(0.561222271706646,0.967776152792487),
 .UNSPECIFIED.)
CURVE()
GEOMETRIC_REPRESENTATION_ITEM()
RATIONAL_B_SPLINE_CURVE((1.56483193275875,1.68587210399417,1.68587210399417))
REPRESENTATION_ITEM('')
);
#216=(
BOUNDED_CURVE()
B_SPLINE_CURVE(2,(#5341,#5342,#5343),.UNSPECIFIED.,.F.,.F.)
B_SPLINE_CURVE_WITH_KNOTS((3,3),(0.967776152792487,1.37433003387833),
 .UNSPECIFIED.)
CURVE()
GEOMETRIC_REPRESENTATION_ITEM()
RATIONAL_B_SPLINE_CURVE((1.68587210399417,1.68587210399417,1.56483193275875))
REPRESENTATION_ITEM('')
);
#217=B_SPLINE_CURVE_WITH_KNOTS('',3,(#4935,#4936,#4937,#4938,#4939,#4940),
 .UNSPECIFIED.,.F.,.F.,(4,2,4),(0.00245247880191636,0.003676905084148,0.00490133136637964),
 .UNSPECIFIED.);
#218=B_SPLINE_CURVE_WITH_KNOTS('',3,(#4942,#4943,#4944,#4945,#4946,#4947,
#4948,#4949,#4950,#4951,#4952,#4953,#4954,#4955,#4956,#4957,#4958,#4959,
#4960,#4961,#4962,#4963,#4964,#4965,#4966,#4967,#4968,#4969,#4970,#4971,
#4972),.UNSPECIFIED.,.F.,.F.,(4,3,3,3,3,3,3,3,3,3,4),(5.67844053276549E-16,
0.000695855432601809,0.00134041800879398,0.00193528387732779,0.00245066568318982,
0.00246968402304892,0.00288934416296891,0.0033283699935918,0.00367599852478473,
0.00430462464290023,0.00490133136636978),.UNSPECIFIED.);
#219=B_SPLINE_CURVE_WITH_KNOTS('',3,(#4974,#4975,#4976,#4977,#4978,#4979,
#4980,#4981,#4982,#4983,#4984,#4985,#4986,#4987,#4988,#4989,#4990,#4991,
#4992,#4993,#4994,#4995,#4996,#4997,#4998,#4999,#5000,#5001,#5002,#5003,
#5004),.UNSPECIFIED.,.F.,.F.,(4,3,3,3,3,3,3,3,3,3,4),(8.85358667444219E-15,
0.000695855432697135,0.0013404180089634,0.00193528387756669,0.00245066568318982,
0.00246968402304891,0.00288934416297983,0.00332836999361881,0.00367599852478473,
0.00430462464295834,0.00490133136637964),.UNSPECIFIED.);
#220=B_SPLINE_CURVE_WITH_KNOTS('',3,(#5006,#5007,#5008,#5009,#5010,#5011,
#5012,#5013,#5014,#5015,#5016,#5017,#5018),.UNSPECIFIED.,.F.,.F.,(4,3,3,
3,4),(8.11127826823332E-15,0.000689795867694038,0.00132892982254773,0.00191855771040346,
0.00245247880191638),.UNSPECIFIED.);
#221=B_SPLINE_CURVE_WITH_KNOTS('',3,(#5020,#5021,#5022,#5023,#5024,#5025),
 .UNSPECIFIED.,.F.,.F.,(4,2,4),(0.00245247880191638,0.00367690508414801,
0.00490133136637964),.UNSPECIFIED.);
#222=B_SPLINE_CURVE_WITH_KNOTS('',3,(#5027,#5028,#5029,#5030,#5031,#5032,
#5033,#5034,#5035,#5036,#5037,#5038,#5039,#5040,#5041,#5042,#5043,#5044,
#5045,#5046,#5047,#5048,#5049,#5050,#5051,#5052,#5053,#5054,#5055,#5056,
#5057),.UNSPECIFIED.,.F.,.F.,(4,3,3,3,3,3,3,3,3,3,4),(0.,0.000695855432618481,
0.00134041800882542,0.00193528387737502,0.00245066568318982,0.00246968402304892,
0.00288934416296796,0.003328369993593,0.00367599852478473,0.00430462464290574,
0.00490133136637964),.UNSPECIFIED.);
#223=B_SPLINE_CURVE_WITH_KNOTS('',3,(#5059,#5060,#5061,#5062,#5063,#5064,
#5065,#5066,#5067,#5068,#5069,#5070,#5071,#5072,#5073,#5074,#5075,#5076,
#5077,#5078,#5079,#5080,#5081,#5082,#5083,#5084,#5085,#5086,#5087,#5088,
#5089),.UNSPECIFIED.,.F.,.F.,(4,3,3,3,3,3,3,3,3,3,4),(6.16572492944553E-15,
0.000695855432688955,0.00134041800894962,0.00193528387754702,0.00245066568318982,
0.00246968402304892,0.00288934416297848,0.00332836999361346,0.00367599852478473,
0.00430462464295078,0.00490133136636899),.UNSPECIFIED.);
#224=B_SPLINE_CURVE_WITH_KNOTS('',3,(#5090,#5091,#5092,#5093,#5094,#5095,
#5096,#5097,#5098,#5099,#5100,#5101,#5102),.UNSPECIFIED.,.F.,.F.,(4,3,3,
3,4),(8.40381044765954E-15,0.000702159417341443,0.00135239722254579,0.00195265359751279,
0.00245247880191636),.UNSPECIFIED.);
#225=B_SPLINE_CURVE_WITH_KNOTS('',3,(#5115,#5116,#5117,#5118,#5119,#5120,
#5121,#5122,#5123,#5124,#5125,#5126,#5127,#5128,#5129,#5130,#5131,#5132,
#5133,#5134,#5135,#5136,#5137,#5138,#5139,#5140,#5141,#5142),
 .UNSPECIFIED.,.F.,.F.,(4,3,3,3,3,3,3,3,3,4),(0.,0.000577214184020621,0.0011469145667476,
0.00171936884360262,0.00229182312045765,0.00230940107675851,0.00301372435340778,
0.00346410161513776,0.00418729554271379,0.00461880215351701),
 .UNSPECIFIED.);
#226=B_SPLINE_CURVE_WITH_KNOTS('',3,(#5156,#5157,#5158,#5159,#5160,#5161,
#5162,#5163,#5164,#5165,#5166,#5167,#5168,#5169,#5170,#5171,#5172,#5173,
#5174,#5175,#5176,#5177,#5178,#5179,#5180,#5181,#5182,#5183),
 .UNSPECIFIED.,.F.,.F.,(4,3,3,3,3,3,3,3,3,4),(0.,0.000577214184043689,0.00114691456679992,
0.00171936884362879,0.00229182312045765,0.00230940107675851,0.00301372435351753,
0.00346410161513776,0.00418729554278622,0.00461880215351701),
 .UNSPECIFIED.);
#227=B_SPLINE_CURVE_WITH_KNOTS('',3,(#5195,#5196,#5197,#5198,#5199,#5200,
#5201,#5202,#5203,#5204,#5205,#5206,#5207,#5208,#5209,#5210,#5211,#5212,
#5213,#5214,#5215,#5216,#5217,#5218,#5219,#5220,#5221,#5222),
 .UNSPECIFIED.,.F.,.F.,(4,3,3,3,3,3,3,3,3,4),(0.,0.000577330594159088,0.00114714311141377,
0.00171942025576102,0.00229169740010826,0.00230940107675851,0.00302569686189932,
0.00346410161513776,0.00419584242927921,0.00461880215351701),
 .UNSPECIFIED.);
#228=B_SPLINE_CURVE_WITH_KNOTS('',3,(#5234,#5235,#5236,#5237,#5238,#5239,
#5240,#5241,#5242,#5243,#5244,#5245,#5246,#5247,#5248,#5249,#5250,#5251,
#5252,#5253,#5254,#5255,#5256,#5257,#5258,#5259,#5260,#5261),
 .UNSPECIFIED.,.F.,.F.,(4,3,3,3,3,3,3,3,3,4),(5.64027445225002E-20,0.000577214184015937,
0.00114691456673884,0.00171936884359825,0.00229182312045766,0.00230940107675851,
0.00301372435339581,0.00346410161513776,0.00418729554270106,0.00461880215351701),
 .UNSPECIFIED.);
#229=B_SPLINE_CURVE_WITH_KNOTS('',3,(#5273,#5274,#5275,#5276,#5277,#5278,
#5279,#5280,#5281,#5282,#5283,#5284,#5285,#5286,#5287,#5288,#5289,#5290,
#5291,#5292,#5293,#5294,#5295,#5296,#5297,#5298,#5299,#5300),
 .UNSPECIFIED.,.F.,.F.,(4,3,3,3,3,3,3,3,3,4),(0.,0.000577214184046313,0.00114691456680682,
0.00171936884363224,0.00229182312045766,0.00230940107675851,0.00301372435353412,
0.00346410161513776,0.00418729554279921,0.00461880215351701),
 .UNSPECIFIED.);
#230=B_SPLINE_CURVE_WITH_KNOTS('',3,(#5309,#5310,#5311,#5312,#5313,#5314,
#5315,#5316,#5317,#5318,#5319,#5320,#5321,#5322,#5323,#5324,#5325,#5326,
#5327,#5328,#5329,#5330,#5331,#5332,#5333,#5334,#5335,#5336),
 .UNSPECIFIED.,.F.,.F.,(4,3,3,3,3,3,3,3,3,4),(0.,0.000577241406570222,0.00114696434019859,
0.00171947309771276,0.00229198185522694,0.00230940107675851,0.00300249253020181,
0.00346410161513776,0.00417905459555678,0.00461880215351701),
 .UNSPECIFIED.);
#231=B_SPLINE_CURVE_WITH_KNOTS('',3,(#5376,#5377,#5378,#5379,#5380,#5381,
#5382,#5383,#5384,#5385,#5386,#5387,#5388,#5389,#5390,#5391,#5392,#5393,
#5394,#5395,#5396,#5397,#5398,#5399,#5400,#5401,#5402,#5403),
 .UNSPECIFIED.,.F.,.F.,(4,3,3,3,3,3,3,3,3,4),(-3.64011549240941E-6,7.47064143895679E-5,
0.000141223222716573,0.000200676503540031,0.000206654603400653,0.000259836747040681,
0.000308997427335436,0.000355388984124418,0.000399064790660936,0.000416939475533297),
 .UNSPECIFIED.);
#232=B_SPLINE_CURVE_WITH_KNOTS('',3,(#5404,#5405,#5406,#5407,#5408,#5409,
#5410,#5411,#5412,#5413,#5414,#5415,#5416,#5417,#5418,#5419,#5420,#5421,
#5422,#5423,#5424,#5425,#5426,#5427,#5428),.UNSPECIFIED.,.F.,.F.,(4,3,3,
3,3,3,3,3,4),(1.01092065026796E-8,4.32951812984497E-5,8.98778625374107E-5,
0.000138990149037295,0.00019384384370113,0.000209511744085474,0.000269284051462139,
0.000350197458189693,0.000419023488170948),.UNSPECIFIED.);
#233=B_SPLINE_CURVE_WITH_KNOTS('',3,(#5447,#5448,#5449,#5450,#5451,#5452,
#5453,#5454,#5455,#5456,#5457,#5458,#5459,#5460,#5461,#5462,#5463,#5464,
#5465,#5466,#5467,#5468,#5469,#5470,#5471),.UNSPECIFIED.,.F.,.F.,(4,3,3,
3,3,3,3,3,4),(1.01015226993228E-8,4.32951932790925E-5,8.98778959717681E-5,
0.000138990207648567,0.000193843941248458,0.000209511744085473,0.000269284041837185,
0.000350197471127522,0.000419023488170945),.UNSPECIFIED.);
#234=B_SPLINE_CURVE_WITH_KNOTS('',3,(#5490,#5491,#5492,#5493,#5494,#5495,
#5496,#5497,#5498,#5499,#5500,#5501,#5502,#5503,#5504,#5505,#5506,#5507,
#5508,#5509,#5510,#5511,#5512,#5513,#5514,#5515,#5516,#5517),
 .UNSPECIFIED.,.F.,.F.,(4,3,3,3,3,3,3,3,3,4),(-3.6401154924107E-6,7.47064416297961E-5,
0.000141223236270614,0.000200676508381646,0.000206654603400652,0.000259836793512798,
0.00030899750605435,0.000355389089154961,0.000399064922535254,0.000416939183220073),
 .UNSPECIFIED.);
#235=B_SPLINE_CURVE_WITH_KNOTS('',3,(#5536,#5537,#5538,#5539,#5540,#5541,
#5542,#5543,#5544,#5545,#5546,#5547,#5548,#5549,#5550,#5551,#5552,#5553,
#5554,#5555,#5556,#5557,#5558,#5559,#5560),.UNSPECIFIED.,.F.,.F.,(4,3,3,
3,3,3,3,3,4),(1.04031327899438E-8,4.32954865334447E-5,8.98781822906502E-5,
0.000138990488526855,0.000193844203201864,0.000209511744085473,0.000269284051462561,
0.000350197458172102,0.000419023488170946),.UNSPECIFIED.);
#236=B_SPLINE_CURVE_WITH_KNOTS('',3,(#5579,#5580,#5581,#5582,#5583,#5584,
#5585,#5586,#5587,#5588,#5589,#5590,#5591,#5592,#5593,#5594,#5595,#5596,
#5597,#5598,#5599,#5600,#5601,#5602,#5603,#5604,#5605,#5606),
 .UNSPECIFIED.,.F.,.F.,(4,3,3,3,3,3,3,3,3,4),(-3.64011549240717E-6,7.47064143979229E-5,
0.000141223222725022,0.000200676503549095,0.000206654603400655,0.000259836754628317,
0.000308997440091673,0.000355389000691412,0.0003990648128455,0.00041693917497655),
 .UNSPECIFIED.);
#237=CONICAL_SURFACE('',#3247,2.042,1.04719755119659);
#238=CONICAL_SURFACE('',#3267,2.055,0.785398163397472);
#239=CONICAL_SURFACE('',#3289,2.5,0.959931088596879);
#240=CONICAL_SURFACE('',#3292,2.06,0.959931088596874);
#241=CONICAL_SURFACE('',#3295,5.56078137864557,1.22173047639605);
#242=CONICAL_SURFACE('',#3316,4.,0.891188651591379);
#243=CONICAL_SURFACE('',#3317,4.,0.891188651591379);
#244=CONICAL_SURFACE('',#3318,4.,0.891188651591379);
#245=CONICAL_SURFACE('',#3319,4.,0.891188651591379);
#246=CONICAL_SURFACE('',#3320,4.,0.891188651591379);
#247=CONICAL_SURFACE('',#3321,4.,0.891188651591379);
#248=TOROIDAL_SURFACE('',#3187,13.3,0.200000000000003);
#249=TOROIDAL_SURFACE('',#3193,13.3,0.200000000000003);
#250=TOROIDAL_SURFACE('',#3204,11.75,1.05);
#251=TOROIDAL_SURFACE('',#3208,10.2,0.200000000000003);
#252=TOROIDAL_SURFACE('',#3214,10.2,0.200000000000003);
#253=TOROIDAL_SURFACE('',#3223,11.75,1.05);
#254=TOROIDAL_SURFACE('',#3254,4.,0.25);
#255=TOROIDAL_SURFACE('',#3258,2.7,0.2);
#256=TOROIDAL_SURFACE('',#3298,5.38445439793712,0.51554560206288);
#257=SHAPE_REPRESENTATION_RELATIONSHIP('SRR','None',#5758,#264);
#258=SHAPE_REPRESENTATION_RELATIONSHIP('SRR','None',#5759,#265);
#259=SHAPE_REPRESENTATION_RELATIONSHIP('SRR','None',#5760,#266);
#260=SHAPE_REPRESENTATION_RELATIONSHIP('SRR','None',#5761,#267);
#261=SHAPE_REPRESENTATION_RELATIONSHIP('SRR','None',#5762,#268);
#262=SHAPE_REPRESENTATION_RELATIONSHIP('SRR','None',#5763,#269);
#263=SHAPE_REPRESENTATION_RELATIONSHIP('SRR','None',#5764,#270);
#264=ADVANCED_BREP_SHAPE_REPRESENTATION('',(#278),#5682);
#265=ADVANCED_BREP_SHAPE_REPRESENTATION('',(#279),#5683);
#266=ADVANCED_BREP_SHAPE_REPRESENTATION('',(#280),#5684);
#267=ADVANCED_BREP_SHAPE_REPRESENTATION('',(#281),#5685);
#268=ADVANCED_BREP_SHAPE_REPRESENTATION('',(#282),#5686);
#269=ADVANCED_BREP_SHAPE_REPRESENTATION('',(#283),#5687);
#270=ADVANCED_BREP_SHAPE_REPRESENTATION('',(#284),#5688);
#271=STYLED_ITEM('',(#5802),#278);
#272=STYLED_ITEM('',(#5803),#279);
#273=STYLED_ITEM('',(#5804),#280);
#274=STYLED_ITEM('',(#5805),#281);
#275=STYLED_ITEM('',(#5804),#282);
#276=STYLED_ITEM('',(#5806),#283);
#277=STYLED_ITEM('',(#5806),#284);
#278=MANIFOLD_SOLID_BREP('Body1',#2961);
#279=MANIFOLD_SOLID_BREP('Body1',#2962);
#280=MANIFOLD_SOLID_BREP('Body1',#2963);
#281=MANIFOLD_SOLID_BREP('Body1',#2964);
#282=MANIFOLD_SOLID_BREP('Body1',#2965);
#283=MANIFOLD_SOLID_BREP('Body1',#2966);
#284=MANIFOLD_SOLID_BREP('Body1',#2967);
#285=FACE_BOUND('',#615,.T.);
#286=FACE_BOUND('',#616,.T.);
#287=FACE_BOUND('',#617,.T.);
#288=FACE_BOUND('',#618,.T.);
#289=FACE_BOUND('',#619,.T.);
#290=FACE_BOUND('',#621,.T.);
#291=FACE_BOUND('',#622,.T.);
#292=FACE_BOUND('',#623,.T.);
#293=FACE_BOUND('',#624,.T.);
#294=FACE_BOUND('',#625,.T.);
#295=FACE_BOUND('',#628,.T.);
#296=FACE_BOUND('',#629,.T.);
#297=FACE_BOUND('',#630,.T.);
#298=FACE_BOUND('',#631,.T.);
#299=FACE_BOUND('',#632,.T.);
#300=FACE_BOUND('',#633,.T.);
#301=FACE_BOUND('',#634,.T.);
#302=FACE_BOUND('',#635,.T.);
#303=FACE_BOUND('',#636,.T.);
#304=FACE_BOUND('',#637,.T.);
#305=FACE_BOUND('',#642,.T.);
#306=FACE_BOUND('',#644,.T.);
#307=FACE_BOUND('',#647,.T.);
#308=FACE_BOUND('',#649,.T.);
#309=FACE_BOUND('',#682,.T.);
#310=FACE_BOUND('',#683,.T.);
#311=FACE_BOUND('',#684,.T.);
#312=FACE_BOUND('',#685,.T.);
#313=FACE_BOUND('',#686,.T.);
#314=FACE_BOUND('',#687,.T.);
#315=FACE_BOUND('',#689,.T.);
#316=FACE_BOUND('',#690,.T.);
#317=FACE_BOUND('',#691,.T.);
#318=FACE_BOUND('',#692,.T.);
#319=FACE_BOUND('',#693,.T.);
#320=FACE_BOUND('',#694,.T.);
#321=FACE_BOUND('',#697,.T.);
#322=FACE_BOUND('',#698,.T.);
#323=FACE_BOUND('',#699,.T.);
#324=FACE_BOUND('',#700,.T.);
#325=FACE_BOUND('',#701,.T.);
#326=FACE_BOUND('',#703,.T.);
#327=FACE_BOUND('',#704,.T.);
#328=FACE_BOUND('',#705,.T.);
#329=FACE_BOUND('',#706,.T.);
#330=FACE_BOUND('',#707,.T.);
#331=FACE_BOUND('',#748,.T.);
#332=FACE_BOUND('',#750,.T.);
#333=FACE_BOUND('',#752,.T.);
#334=FACE_BOUND('',#754,.T.);
#335=FACE_BOUND('',#760,.T.);
#336=FACE_BOUND('',#762,.T.);
#337=FACE_BOUND('',#764,.T.);
#338=FACE_BOUND('',#766,.T.);
#339=FACE_BOUND('',#774,.T.);
#340=FACE_BOUND('',#777,.T.);
#341=FACE_BOUND('',#803,.T.);
#342=FACE_BOUND('',#805,.T.);
#343=PLANE('',#3084);
#344=PLANE('',#3085);
#345=PLANE('',#3086);
#346=PLANE('',#3087);
#347=PLANE('',#3088);
#348=PLANE('',#3089);
#349=PLANE('',#3090);
#350=PLANE('',#3091);
#351=PLANE('',#3092);
#352=PLANE('',#3094);
#353=PLANE('',#3096);
#354=PLANE('',#3097);
#355=PLANE('',#3099);
#356=PLANE('',#3101);
#357=PLANE('',#3102);
#358=PLANE('',#3103);
#359=PLANE('',#3106);
#360=PLANE('',#3107);
#361=PLANE('',#3124);
#362=PLANE('',#3125);
#363=PLANE('',#3126);
#364=PLANE('',#3127);
#365=PLANE('',#3128);
#366=PLANE('',#3129);
#367=PLANE('',#3130);
#368=PLANE('',#3131);
#369=PLANE('',#3132);
#370=PLANE('',#3133);
#371=PLANE('',#3134);
#372=PLANE('',#3135);
#373=PLANE('',#3136);
#374=PLANE('',#3137);
#375=PLANE('',#3138);
#376=PLANE('',#3139);
#377=PLANE('',#3140);
#378=PLANE('',#3141);
#379=PLANE('',#3142);
#380=PLANE('',#3143);
#381=PLANE('',#3144);
#382=PLANE('',#3145);
#383=PLANE('',#3146);
#384=PLANE('',#3147);
#385=PLANE('',#3148);
#386=PLANE('',#3149);
#387=PLANE('',#3150);
#388=PLANE('',#3151);
#389=PLANE('',#3152);
#390=PLANE('',#3153);
#391=PLANE('',#3154);
#392=PLANE('',#3155);
#393=PLANE('',#3168);
#394=PLANE('',#3169);
#395=PLANE('',#3170);
#396=PLANE('',#3171);
#397=PLANE('',#3172);
#398=PLANE('',#3173);
#399=PLANE('',#3174);
#400=PLANE('',#3175);
#401=PLANE('',#3176);
#402=PLANE('',#3177);
#403=PLANE('',#3178);
#404=PLANE('',#3179);
#405=PLANE('',#3180);
#406=PLANE('',#3181);
#407=PLANE('',#3182);
#408=PLANE('',#3183);
#409=PLANE('',#3184);
#410=PLANE('',#3185);
#411=PLANE('',#3225);
#412=PLANE('',#3226);
#413=PLANE('',#3227);
#414=PLANE('',#3228);
#415=PLANE('',#3242);
#416=PLANE('',#3243);
#417=PLANE('',#3244);
#418=PLANE('',#3245);
#419=PLANE('',#3269);
#420=PLANE('',#3270);
#421=PLANE('',#3271);
#422=PLANE('',#3272);
#423=PLANE('',#3273);
#424=PLANE('',#3274);
#425=PLANE('',#3275);
#426=PLANE('',#3276);
#427=PLANE('',#3277);
#428=PLANE('',#3278);
#429=PLANE('',#3279);
#430=PLANE('',#3280);
#431=PLANE('',#3281);
#432=PLANE('',#3282);
#433=PLANE('',#3283);
#434=PLANE('',#3302);
#435=PLANE('',#3303);
#436=PLANE('',#3304);
#437=PLANE('',#3305);
#438=PLANE('',#3306);
#439=PLANE('',#3307);
#440=PLANE('',#3308);
#441=PLANE('',#3315);
#442=FACE_OUTER_BOUND('',#601,.T.);
#443=FACE_OUTER_BOUND('',#602,.T.);
#444=FACE_OUTER_BOUND('',#603,.T.);
#445=FACE_OUTER_BOUND('',#604,.T.);
#446=FACE_OUTER_BOUND('',#605,.T.);
#447=FACE_OUTER_BOUND('',#606,.T.);
#448=FACE_OUTER_BOUND('',#607,.T.);
#449=FACE_OUTER_BOUND('',#608,.T.);
#450=FACE_OUTER_BOUND('',#609,.T.);
#451=FACE_OUTER_BOUND('',#610,.T.);
#452=FACE_OUTER_BOUND('',#611,.T.);
#453=FACE_OUTER_BOUND('',#612,.T.);
#454=FACE_OUTER_BOUND('',#613,.T.);
#455=FACE_OUTER_BOUND('',#614,.T.);
#456=FACE_OUTER_BOUND('',#620,.T.);
#457=FACE_OUTER_BOUND('',#626,.T.);
#458=FACE_OUTER_BOUND('',#627,.T.);
#459=FACE_OUTER_BOUND('',#638,.T.);
#460=FACE_OUTER_BOUND('',#639,.T.);
#461=FACE_OUTER_BOUND('',#640,.T.);
#462=FACE_OUTER_BOUND('',#641,.T.);
#463=FACE_OUTER_BOUND('',#643,.T.);
#464=FACE_OUTER_BOUND('',#645,.T.);
#465=FACE_OUTER_BOUND('',#646,.T.);
#466=FACE_OUTER_BOUND('',#648,.T.);
#467=FACE_OUTER_BOUND('',#650,.T.);
#468=FACE_OUTER_BOUND('',#651,.T.);
#469=FACE_OUTER_BOUND('',#652,.T.);
#470=FACE_OUTER_BOUND('',#653,.T.);
#471=FACE_OUTER_BOUND('',#654,.T.);
#472=FACE_OUTER_BOUND('',#655,.T.);
#473=FACE_OUTER_BOUND('',#656,.T.);
#474=FACE_OUTER_BOUND('',#657,.T.);
#475=FACE_OUTER_BOUND('',#658,.T.);
#476=FACE_OUTER_BOUND('',#659,.T.);
#477=FACE_OUTER_BOUND('',#660,.T.);
#478=FACE_OUTER_BOUND('',#661,.T.);
#479=FACE_OUTER_BOUND('',#662,.T.);
#480=FACE_OUTER_BOUND('',#663,.T.);
#481=FACE_OUTER_BOUND('',#664,.T.);
#482=FACE_OUTER_BOUND('',#665,.T.);
#483=FACE_OUTER_BOUND('',#666,.T.);
#484=FACE_OUTER_BOUND('',#667,.T.);
#485=FACE_OUTER_BOUND('',#668,.T.);
#486=FACE_OUTER_BOUND('',#669,.T.);
#487=FACE_OUTER_BOUND('',#670,.T.);
#488=FACE_OUTER_BOUND('',#671,.T.);
#489=FACE_OUTER_BOUND('',#672,.T.);
#490=FACE_OUTER_BOUND('',#673,.T.);
#491=FACE_OUTER_BOUND('',#674,.T.);
#492=FACE_OUTER_BOUND('',#675,.T.);
#493=FACE_OUTER_BOUND('',#676,.T.);
#494=FACE_OUTER_BOUND('',#677,.T.);
#495=FACE_OUTER_BOUND('',#678,.T.);
#496=FACE_OUTER_BOUND('',#679,.T.);
#497=FACE_OUTER_BOUND('',#680,.T.);
#498=FACE_OUTER_BOUND('',#681,.T.);
#499=FACE_OUTER_BOUND('',#688,.T.);
#500=FACE_OUTER_BOUND('',#695,.T.);
#501=FACE_OUTER_BOUND('',#696,.T.);
#502=FACE_OUTER_BOUND('',#702,.T.);
#503=FACE_OUTER_BOUND('',#708,.T.);
#504=FACE_OUTER_BOUND('',#709,.T.);
#505=FACE_OUTER_BOUND('',#710,.T.);
#506=FACE_OUTER_BOUND('',#711,.T.);
#507=FACE_OUTER_BOUND('',#712,.T.);
#508=FACE_OUTER_BOUND('',#713,.T.);
#509=FACE_OUTER_BOUND('',#714,.T.);
#510=FACE_OUTER_BOUND('',#715,.T.);
#511=FACE_OUTER_BOUND('',#716,.T.);
#512=FACE_OUTER_BOUND('',#717,.T.);
#513=FACE_OUTER_BOUND('',#718,.T.);
#514=FACE_OUTER_BOUND('',#719,.T.);
#515=FACE_OUTER_BOUND('',#720,.T.);
#516=FACE_OUTER_BOUND('',#721,.T.);
#517=FACE_OUTER_BOUND('',#722,.T.);
#518=FACE_OUTER_BOUND('',#723,.T.);
#519=FACE_OUTER_BOUND('',#724,.T.);
#520=FACE_OUTER_BOUND('',#725,.T.);
#521=FACE_OUTER_BOUND('',#726,.T.);
#522=FACE_OUTER_BOUND('',#727,.T.);
#523=FACE_OUTER_BOUND('',#728,.T.);
#524=FACE_OUTER_BOUND('',#729,.T.);
#525=FACE_OUTER_BOUND('',#730,.T.);
#526=FACE_OUTER_BOUND('',#731,.T.);
#527=FACE_OUTER_BOUND('',#732,.T.);
#528=FACE_OUTER_BOUND('',#733,.T.);
#529=FACE_OUTER_BOUND('',#734,.T.);
#530=FACE_OUTER_BOUND('',#735,.T.);
#531=FACE_OUTER_BOUND('',#736,.T.);
#532=FACE_OUTER_BOUND('',#737,.T.);
#533=FACE_OUTER_BOUND('',#738,.T.);
#534=FACE_OUTER_BOUND('',#739,.T.);
#535=FACE_OUTER_BOUND('',#740,.T.);
#536=FACE_OUTER_BOUND('',#741,.T.);
#537=FACE_OUTER_BOUND('',#742,.T.);
#538=FACE_OUTER_BOUND('',#743,.T.);
#539=FACE_OUTER_BOUND('',#744,.T.);
#540=FACE_OUTER_BOUND('',#745,.T.);
#541=FACE_OUTER_BOUND('',#746,.T.);
#542=FACE_OUTER_BOUND('',#747,.T.);
#543=FACE_OUTER_BOUND('',#749,.T.);
#544=FACE_OUTER_BOUND('',#751,.T.);
#545=FACE_OUTER_BOUND('',#753,.T.);
#546=FACE_OUTER_BOUND('',#755,.T.);
#547=FACE_OUTER_BOUND('',#756,.T.);
#548=FACE_OUTER_BOUND('',#757,.T.);
#549=FACE_OUTER_BOUND('',#758,.T.);
#550=FACE_OUTER_BOUND('',#759,.T.);
#551=FACE_OUTER_BOUND('',#761,.T.);
#552=FACE_OUTER_BOUND('',#763,.T.);
#553=FACE_OUTER_BOUND('',#765,.T.);
#554=FACE_OUTER_BOUND('',#767,.T.);
#555=FACE_OUTER_BOUND('',#768,.T.);
#556=FACE_OUTER_BOUND('',#769,.T.);
#557=FACE_OUTER_BOUND('',#770,.T.);
#558=FACE_OUTER_BOUND('',#771,.T.);
#559=FACE_OUTER_BOUND('',#772,.T.);
#560=FACE_OUTER_BOUND('',#773,.T.);
#561=FACE_OUTER_BOUND('',#775,.T.);
#562=FACE_OUTER_BOUND('',#776,.T.);
#563=FACE_OUTER_BOUND('',#778,.T.);
#564=FACE_OUTER_BOUND('',#779,.T.);
#565=FACE_OUTER_BOUND('',#780,.T.);
#566=FACE_OUTER_BOUND('',#781,.T.);
#567=FACE_OUTER_BOUND('',#782,.T.);
#568=FACE_OUTER_BOUND('',#783,.T.);
#569=FACE_OUTER_BOUND('',#784,.T.);
#570=FACE_OUTER_BOUND('',#785,.T.);
#571=FACE_OUTER_BOUND('',#786,.T.);
#572=FACE_OUTER_BOUND('',#787,.T.);
#573=FACE_OUTER_BOUND('',#788,.T.);
#574=FACE_OUTER_BOUND('',#789,.T.);
#575=FACE_OUTER_BOUND('',#790,.T.);
#576=FACE_OUTER_BOUND('',#791,.T.);
#577=FACE_OUTER_BOUND('',#792,.T.);
#578=FACE_OUTER_BOUND('',#793,.T.);
#579=FACE_OUTER_BOUND('',#794,.T.);
#580=FACE_OUTER_BOUND('',#795,.T.);
#581=FACE_OUTER_BOUND('',#796,.T.);
#582=FACE_OUTER_BOUND('',#797,.T.);
#583=FACE_OUTER_BOUND('',#798,.T.);
#584=FACE_OUTER_BOUND('',#799,.T.);
#585=FACE_OUTER_BOUND('',#800,.T.);
#586=FACE_OUTER_BOUND('',#801,.T.);
#587=FACE_OUTER_BOUND('',#802,.T.);
#588=FACE_OUTER_BOUND('',#804,.T.);
#589=FACE_OUTER_BOUND('',#806,.T.);
#590=FACE_OUTER_BOUND('',#807,.T.);
#591=FACE_OUTER_BOUND('',#808,.T.);
#592=FACE_OUTER_BOUND('',#809,.T.);
#593=FACE_OUTER_BOUND('',#810,.T.);
#594=FACE_OUTER_BOUND('',#811,.T.);
#595=FACE_OUTER_BOUND('',#812,.T.);
#596=FACE_OUTER_BOUND('',#813,.T.);
#597=FACE_OUTER_BOUND('',#814,.T.);
#598=FACE_OUTER_BOUND('',#815,.T.);
#599=FACE_OUTER_BOUND('',#816,.T.);
#600=FACE_OUTER_BOUND('',#817,.T.);
#601=EDGE_LOOP('',(#2012,#2013,#2014,#2015));
#602=EDGE_LOOP('',(#2016,#2017,#2018,#2019));
#603=EDGE_LOOP('',(#2020,#2021,#2022,#2023));
#604=EDGE_LOOP('',(#2024,#2025,#2026,#2027));
#605=EDGE_LOOP('',(#2028,#2029,#2030,#2031));
#606=EDGE_LOOP('',(#2032,#2033,#2034,#2035));
#607=EDGE_LOOP('',(#2036,#2037,#2038,#2039));
#608=EDGE_LOOP('',(#2040,#2041,#2042,#2043));
#609=EDGE_LOOP('',(#2044,#2045,#2046,#2047));
#610=EDGE_LOOP('',(#2048,#2049,#2050,#2051));
#611=EDGE_LOOP('',(#2052,#2053,#2054,#2055));
#612=EDGE_LOOP('',(#2056,#2057,#2058,#2059));
#613=EDGE_LOOP('',(#2060,#2061,#2062,#2063));
#614=EDGE_LOOP('',(#2064,#2065,#2066,#2067));
#615=EDGE_LOOP('',(#2068));
#616=EDGE_LOOP('',(#2069));
#617=EDGE_LOOP('',(#2070));
#618=EDGE_LOOP('',(#2071));
#619=EDGE_LOOP('',(#2072));
#620=EDGE_LOOP('',(#2073,#2074,#2075,#2076));
#621=EDGE_LOOP('',(#2077));
#622=EDGE_LOOP('',(#2078));
#623=EDGE_LOOP('',(#2079));
#624=EDGE_LOOP('',(#2080));
#625=EDGE_LOOP('',(#2081));
#626=EDGE_LOOP('',(#2082,#2083,#2084,#2085,#2086,#2087,#2088,#2089,#2090,
#2091,#2092,#2093));
#627=EDGE_LOOP('',(#2094,#2095,#2096,#2097));
#628=EDGE_LOOP('',(#2098));
#629=EDGE_LOOP('',(#2099));
#630=EDGE_LOOP('',(#2100));
#631=EDGE_LOOP('',(#2101));
#632=EDGE_LOOP('',(#2102));
#633=EDGE_LOOP('',(#2103));
#634=EDGE_LOOP('',(#2104));
#635=EDGE_LOOP('',(#2105));
#636=EDGE_LOOP('',(#2106));
#637=EDGE_LOOP('',(#2107));
#638=EDGE_LOOP('',(#2108,#2109,#2110,#2111,#2112,#2113,#2114,#2115,#2116,
#2117,#2118,#2119));
#639=EDGE_LOOP('',(#2120,#2121,#2122,#2123));
#640=EDGE_LOOP('',(#2124,#2125,#2126,#2127));
#641=EDGE_LOOP('',(#2128,#2129,#2130,#2131));
#642=EDGE_LOOP('',(#2132,#2133,#2134,#2135));
#643=EDGE_LOOP('',(#2136,#2137,#2138,#2139));
#644=EDGE_LOOP('',(#2140,#2141,#2142,#2143));
#645=EDGE_LOOP('',(#2144,#2145,#2146,#2147));
#646=EDGE_LOOP('',(#2148,#2149,#2150,#2151));
#647=EDGE_LOOP('',(#2152,#2153,#2154,#2155));
#648=EDGE_LOOP('',(#2156,#2157,#2158,#2159));
#649=EDGE_LOOP('',(#2160,#2161,#2162,#2163));
#650=EDGE_LOOP('',(#2164,#2165,#2166,#2167));
#651=EDGE_LOOP('',(#2168,#2169,#2170,#2171));
#652=EDGE_LOOP('',(#2172,#2173,#2174,#2175));
#653=EDGE_LOOP('',(#2176,#2177,#2178,#2179));
#654=EDGE_LOOP('',(#2180,#2181,#2182,#2183));
#655=EDGE_LOOP('',(#2184,#2185,#2186,#2187));
#656=EDGE_LOOP('',(#2188,#2189,#2190,#2191));
#657=EDGE_LOOP('',(#2192,#2193,#2194,#2195));
#658=EDGE_LOOP('',(#2196,#2197,#2198,#2199));
#659=EDGE_LOOP('',(#2200,#2201,#2202,#2203));
#660=EDGE_LOOP('',(#2204,#2205,#2206,#2207));
#661=EDGE_LOOP('',(#2208,#2209,#2210,#2211));
#662=EDGE_LOOP('',(#2212,#2213,#2214,#2215));
#663=EDGE_LOOP('',(#2216,#2217,#2218,#2219));
#664=EDGE_LOOP('',(#2220,#2221,#2222,#2223));
#665=EDGE_LOOP('',(#2224,#2225,#2226,#2227));
#666=EDGE_LOOP('',(#2228,#2229,#2230,#2231));
#667=EDGE_LOOP('',(#2232,#2233,#2234,#2235));
#668=EDGE_LOOP('',(#2236,#2237,#2238,#2239));
#669=EDGE_LOOP('',(#2240,#2241,#2242,#2243));
#670=EDGE_LOOP('',(#2244,#2245,#2246,#2247));
#671=EDGE_LOOP('',(#2248,#2249,#2250,#2251));
#672=EDGE_LOOP('',(#2252,#2253,#2254,#2255));
#673=EDGE_LOOP('',(#2256,#2257,#2258,#2259));
#674=EDGE_LOOP('',(#2260,#2261,#2262,#2263));
#675=EDGE_LOOP('',(#2264,#2265,#2266,#2267));
#676=EDGE_LOOP('',(#2268,#2269,#2270,#2271));
#677=EDGE_LOOP('',(#2272,#2273,#2274,#2275));
#678=EDGE_LOOP('',(#2276,#2277,#2278,#2279,#2280,#2281));
#679=EDGE_LOOP('',(#2282,#2283,#2284,#2285,#2286,#2287));
#680=EDGE_LOOP('',(#2288,#2289,#2290,#2291));
#681=EDGE_LOOP('',(#2292,#2293,#2294,#2295));
#682=EDGE_LOOP('',(#2296,#2297,#2298,#2299));
#683=EDGE_LOOP('',(#2300,#2301,#2302,#2303));
#684=EDGE_LOOP('',(#2304,#2305,#2306,#2307));
#685=EDGE_LOOP('',(#2308,#2309,#2310,#2311));
#686=EDGE_LOOP('',(#2312,#2313,#2314,#2315));
#687=EDGE_LOOP('',(#2316,#2317,#2318,#2319));
#688=EDGE_LOOP('',(#2320,#2321,#2322,#2323));
#689=EDGE_LOOP('',(#2324,#2325,#2326,#2327));
#690=EDGE_LOOP('',(#2328,#2329,#2330,#2331));
#691=EDGE_LOOP('',(#2332,#2333,#2334,#2335));
#692=EDGE_LOOP('',(#2336,#2337,#2338,#2339));
#693=EDGE_LOOP('',(#2340,#2341,#2342,#2343));
#694=EDGE_LOOP('',(#2344,#2345,#2346,#2347));
#695=EDGE_LOOP('',(#2348,#2349,#2350,#2351));
#696=EDGE_LOOP('',(#2352,#2353,#2354,#2355));
#697=EDGE_LOOP('',(#2356));
#698=EDGE_LOOP('',(#2357));
#699=EDGE_LOOP('',(#2358));
#700=EDGE_LOOP('',(#2359));
#701=EDGE_LOOP('',(#2360));
#702=EDGE_LOOP('',(#2361,#2362,#2363,#2364));
#703=EDGE_LOOP('',(#2365));
#704=EDGE_LOOP('',(#2366));
#705=EDGE_LOOP('',(#2367));
#706=EDGE_LOOP('',(#2368));
#707=EDGE_LOOP('',(#2369));
#708=EDGE_LOOP('',(#2370,#2371,#2372,#2373));
#709=EDGE_LOOP('',(#2374,#2375,#2376,#2377));
#710=EDGE_LOOP('',(#2378,#2379,#2380,#2381));
#711=EDGE_LOOP('',(#2382,#2383,#2384,#2385));
#712=EDGE_LOOP('',(#2386,#2387,#2388,#2389));
#713=EDGE_LOOP('',(#2390,#2391,#2392,#2393));
#714=EDGE_LOOP('',(#2394,#2395,#2396,#2397));
#715=EDGE_LOOP('',(#2398,#2399,#2400,#2401));
#716=EDGE_LOOP('',(#2402,#2403,#2404,#2405,#2406,#2407,#2408,#2409,#2410,
#2411,#2412,#2413));
#717=EDGE_LOOP('',(#2414,#2415,#2416));
#718=EDGE_LOOP('',(#2417,#2418));
#719=EDGE_LOOP('',(#2419,#2420));
#720=EDGE_LOOP('',(#2421,#2422));
#721=EDGE_LOOP('',(#2423,#2424,#2425));
#722=EDGE_LOOP('',(#2426,#2427));
#723=EDGE_LOOP('',(#2428,#2429));
#724=EDGE_LOOP('',(#2430,#2431));
#725=EDGE_LOOP('',(#2432,#2433,#2434,#2435));
#726=EDGE_LOOP('',(#2436,#2437,#2438,#2439));
#727=EDGE_LOOP('',(#2440,#2441,#2442,#2443));
#728=EDGE_LOOP('',(#2444,#2445,#2446,#2447));
#729=EDGE_LOOP('',(#2448,#2449,#2450,#2451));
#730=EDGE_LOOP('',(#2452,#2453,#2454,#2455));
#731=EDGE_LOOP('',(#2456,#2457,#2458,#2459));
#732=EDGE_LOOP('',(#2460,#2461,#2462,#2463));
#733=EDGE_LOOP('',(#2464,#2465,#2466,#2467));
#734=EDGE_LOOP('',(#2468,#2469,#2470,#2471));
#735=EDGE_LOOP('',(#2472,#2473,#2474,#2475));
#736=EDGE_LOOP('',(#2476,#2477,#2478,#2479));
#737=EDGE_LOOP('',(#2480,#2481,#2482,#2483));
#738=EDGE_LOOP('',(#2484,#2485,#2486,#2487,#2488));
#739=EDGE_LOOP('',(#2489,#2490,#2491,#2492,#2493));
#740=EDGE_LOOP('',(#2494,#2495,#2496,#2497,#2498,#2499));
#741=EDGE_LOOP('',(#2500,#2501,#2502,#2503));
#742=EDGE_LOOP('',(#2504,#2505,#2506,#2507));
#743=EDGE_LOOP('',(#2508,#2509,#2510,#2511));
#744=EDGE_LOOP('',(#2512,#2513,#2514,#2515,#2516));
#745=EDGE_LOOP('',(#2517,#2518,#2519,#2520,#2521));
#746=EDGE_LOOP('',(#2522,#2523,#2524,#2525,#2526,#2527));
#747=EDGE_LOOP('',(#2528));
#748=EDGE_LOOP('',(#2529));
#749=EDGE_LOOP('',(#2530));
#750=EDGE_LOOP('',(#2531));
#751=EDGE_LOOP('',(#2532));
#752=EDGE_LOOP('',(#2533));
#753=EDGE_LOOP('',(#2534));
#754=EDGE_LOOP('',(#2535));
#755=EDGE_LOOP('',(#2536,#2537,#2538,#2539));
#756=EDGE_LOOP('',(#2540,#2541,#2542,#2543));
#757=EDGE_LOOP('',(#2544,#2545,#2546,#2547));
#758=EDGE_LOOP('',(#2548,#2549,#2550,#2551));
#759=EDGE_LOOP('',(#2552));
#760=EDGE_LOOP('',(#2553));
#761=EDGE_LOOP('',(#2554));
#762=EDGE_LOOP('',(#2555));
#763=EDGE_LOOP('',(#2556));
#764=EDGE_LOOP('',(#2557));
#765=EDGE_LOOP('',(#2558));
#766=EDGE_LOOP('',(#2559));
#767=EDGE_LOOP('',(#2560,#2561,#2562,#2563,#2564,#2565,#2566,#2567));
#768=EDGE_LOOP('',(#2568,#2569,#2570,#2571));
#769=EDGE_LOOP('',(#2572,#2573,#2574,#2575,#2576));
#770=EDGE_LOOP('',(#2577,#2578,#2579,#2580));
#771=EDGE_LOOP('',(#2581,#2582,#2583,#2584,#2585));
#772=EDGE_LOOP('',(#2586,#2587,#2588,#2589));
#773=EDGE_LOOP('',(#2590));
#774=EDGE_LOOP('',(#2591,#2592,#2593,#2594,#2595,#2596));
#775=EDGE_LOOP('',(#2597));
#776=EDGE_LOOP('',(#2598));
#777=EDGE_LOOP('',(#2599));
#778=EDGE_LOOP('',(#2600,#2601,#2602,#2603,#2604));
#779=EDGE_LOOP('',(#2605,#2606,#2607,#2608,#2609));
#780=EDGE_LOOP('',(#2610,#2611,#2612,#2613,#2614));
#781=EDGE_LOOP('',(#2615,#2616,#2617,#2618,#2619));
#782=EDGE_LOOP('',(#2620,#2621,#2622,#2623,#2624));
#783=EDGE_LOOP('',(#2625,#2626,#2627,#2628,#2629));
#784=EDGE_LOOP('',(#2630,#2631,#2632));
#785=EDGE_LOOP('',(#2633,#2634,#2635));
#786=EDGE_LOOP('',(#2636,#2637,#2638));
#787=EDGE_LOOP('',(#2639,#2640,#2641));
#788=EDGE_LOOP('',(#2642,#2643,#2644));
#789=EDGE_LOOP('',(#2645,#2646,#2647));
#790=EDGE_LOOP('',(#2648,#2649,#2650,#2651,#2652));
#791=EDGE_LOOP('',(#2653,#2654,#2655,#2656,#2657,#2658));
#792=EDGE_LOOP('',(#2659,#2660,#2661,#2662));
#793=EDGE_LOOP('',(#2663,#2664,#2665,#2666,#2667,#2668,#2669,#2670,#2671,
#2672,#2673,#2674));
#794=EDGE_LOOP('',(#2675,#2676,#2677,#2678,#2679));
#795=EDGE_LOOP('',(#2680,#2681,#2682,#2683,#2684));
#796=EDGE_LOOP('',(#2685,#2686,#2687,#2688,#2689));
#797=EDGE_LOOP('',(#2690,#2691,#2692,#2693,#2694));
#798=EDGE_LOOP('',(#2695,#2696,#2697,#2698,#2699));
#799=EDGE_LOOP('',(#2700,#2701,#2702,#2703,#2704));
#800=EDGE_LOOP('',(#2705,#2706,#2707,#2708,#2709));
#801=EDGE_LOOP('',(#2710,#2711,#2712,#2713,#2714));
#802=EDGE_LOOP('',(#2715,#2716,#2717,#2718,#2719,#2720));
#803=EDGE_LOOP('',(#2721));
#804=EDGE_LOOP('',(#2722));
#805=EDGE_LOOP('',(#2723));
#806=EDGE_LOOP('',(#2724,#2725,#2726));
#807=EDGE_LOOP('',(#2727,#2728,#2729));
#808=EDGE_LOOP('',(#2730,#2731,#2732));
#809=EDGE_LOOP('',(#2733,#2734,#2735));
#810=EDGE_LOOP('',(#2736,#2737,#2738));
#811=EDGE_LOOP('',(#2739,#2740,#2741));
#812=EDGE_LOOP('',(#2742,#2743,#2744,#2745));
#813=EDGE_LOOP('',(#2746,#2747,#2748,#2749));
#814=EDGE_LOOP('',(#2750,#2751,#2752,#2753,#2754));
#815=EDGE_LOOP('',(#2755,#2756,#2757,#2758,#2759));
#816=EDGE_LOOP('',(#2760,#2761,#2762,#2763));
#817=EDGE_LOOP('',(#2764,#2765,#2766,#2767));
#818=LINE('',#4253,#1049);
#819=LINE('',#4256,#1050);
#820=LINE('',#4262,#1051);
#821=LINE('',#4265,#1052);
#822=LINE('',#4270,#1053);
#823=LINE('',#4276,#1054);
#824=LINE('',#4282,#1055);
#825=LINE('',#4288,#1056);
#826=LINE('',#4294,#1057);
#827=LINE('',#4300,#1058);
#828=LINE('',#4306,#1059);
#829=LINE('',#4312,#1060);
#830=LINE('',#4318,#1061);
#831=LINE('',#4324,#1062);
#832=LINE('',#4329,#1063);
#833=LINE('',#4331,#1064);
#834=LINE('',#4333,#1065);
#835=LINE('',#4334,#1066);
#836=LINE('',#4338,#1067);
#837=LINE('',#4340,#1068);
#838=LINE('',#4342,#1069);
#839=LINE('',#4343,#1070);
#840=LINE('',#4347,#1071);
#841=LINE('',#4349,#1072);
#842=LINE('',#4351,#1073);
#843=LINE('',#4352,#1074);
#844=LINE('',#4355,#1075);
#845=LINE('',#4357,#1076);
#846=LINE('',#4358,#1077);
#847=LINE('',#4360,#1078);
#848=LINE('',#4362,#1079);
#849=LINE('',#4363,#1080);
#850=LINE('',#4365,#1081);
#851=LINE('',#4367,#1082);
#852=LINE('',#4368,#1083);
#853=LINE('',#4371,#1084);
#854=LINE('',#4373,#1085);
#855=LINE('',#4374,#1086);
#856=LINE('',#4376,#1087);
#857=LINE('',#4378,#1088);
#858=LINE('',#4380,#1089);
#859=LINE('',#4381,#1090);
#860=LINE('',#4383,#1091);
#861=LINE('',#4385,#1092);
#862=LINE('',#4386,#1093);
#863=LINE('',#4387,#1094);
#864=LINE('',#4391,#1095);
#865=LINE('',#4393,#1096);
#866=LINE('',#4396,#1097);
#867=LINE('',#4398,#1098);
#868=LINE('',#4402,#1099);
#869=LINE('',#4403,#1100);
#870=LINE('',#4406,#1101);
#871=LINE('',#4408,#1102);
#872=LINE('',#4411,#1103);
#873=LINE('',#4413,#1104);
#874=LINE('',#4417,#1105);
#875=LINE('',#4418,#1106);
#876=LINE('',#4421,#1107);
#877=LINE('',#4423,#1108);
#878=LINE('',#4426,#1109);
#879=LINE('',#4427,#1110);
#880=LINE('',#4435,#1111);
#881=LINE('',#4441,#1112);
#882=LINE('',#4447,#1113);
#883=LINE('',#4453,#1114);
#884=LINE('',#4459,#1115);
#885=LINE('',#4464,#1116);
#886=LINE('',#4466,#1117);
#887=LINE('',#4468,#1118);
#888=LINE('',#4469,#1119);
#889=LINE('',#4472,#1120);
#890=LINE('',#4474,#1121);
#891=LINE('',#4475,#1122);
#892=LINE('',#4478,#1123);
#893=LINE('',#4480,#1124);
#894=LINE('',#4481,#1125);
#895=LINE('',#4483,#1126);
#896=LINE('',#4484,#1127);
#897=LINE('',#4488,#1128);
#898=LINE('',#4490,#1129);
#899=LINE('',#4492,#1130);
#900=LINE('',#4493,#1131);
#901=LINE('',#4496,#1132);
#902=LINE('',#4498,#1133);
#903=LINE('',#4499,#1134);
#904=LINE('',#4502,#1135);
#905=LINE('',#4504,#1136);
#906=LINE('',#4505,#1137);
#907=LINE('',#4507,#1138);
#908=LINE('',#4508,#1139);
#909=LINE('',#4512,#1140);
#910=LINE('',#4514,#1141);
#911=LINE('',#4516,#1142);
#912=LINE('',#4517,#1143);
#913=LINE('',#4520,#1144);
#914=LINE('',#4522,#1145);
#915=LINE('',#4523,#1146);
#916=LINE('',#4526,#1147);
#917=LINE('',#4528,#1148);
#918=LINE('',#4529,#1149);
#919=LINE('',#4531,#1150);
#920=LINE('',#4532,#1151);
#921=LINE('',#4536,#1152);
#922=LINE('',#4538,#1153);
#923=LINE('',#4540,#1154);
#924=LINE('',#4541,#1155);
#925=LINE('',#4544,#1156);
#926=LINE('',#4546,#1157);
#927=LINE('',#4547,#1158);
#928=LINE('',#4550,#1159);
#929=LINE('',#4552,#1160);
#930=LINE('',#4553,#1161);
#931=LINE('',#4555,#1162);
#932=LINE('',#4556,#1163);
#933=LINE('',#4560,#1164);
#934=LINE('',#4562,#1165);
#935=LINE('',#4564,#1166);
#936=LINE('',#4566,#1167);
#937=LINE('',#4568,#1168);
#938=LINE('',#4569,#1169);
#939=LINE('',#4573,#1170);
#940=LINE('',#4575,#1171);
#941=LINE('',#4577,#1172);
#942=LINE('',#4579,#1173);
#943=LINE('',#4581,#1174);
#944=LINE('',#4582,#1175);
#945=LINE('',#4584,#1176);
#946=LINE('',#4585,#1177);
#947=LINE('',#4587,#1178);
#948=LINE('',#4590,#1179);
#949=LINE('',#4592,#1180);
#950=LINE('',#4594,#1181);
#951=LINE('',#4595,#1182);
#952=LINE('',#4598,#1183);
#953=LINE('',#4600,#1184);
#954=LINE('',#4602,#1185);
#955=LINE('',#4603,#1186);
#956=LINE('',#4605,#1187);
#957=LINE('',#4608,#1188);
#958=LINE('',#4610,#1189);
#959=LINE('',#4612,#1190);
#960=LINE('',#4613,#1191);
#961=LINE('',#4616,#1192);
#962=LINE('',#4618,#1193);
#963=LINE('',#4620,#1194);
#964=LINE('',#4621,#1195);
#965=LINE('',#4623,#1196);
#966=LINE('',#4624,#1197);
#967=LINE('',#4628,#1198);
#968=LINE('',#4629,#1199);
#969=LINE('',#4631,#1200);
#970=LINE('',#4633,#1201);
#971=LINE('',#4636,#1202);
#972=LINE('',#4637,#1203);
#973=LINE('',#4639,#1204);
#974=LINE('',#4641,#1205);
#975=LINE('',#4653,#1206);
#976=LINE('',#4667,#1207);
#977=LINE('',#4669,#1208);
#978=LINE('',#4671,#1209);
#979=LINE('',#4673,#1210);
#980=LINE('',#4675,#1211);
#981=LINE('',#4677,#1212);
#982=LINE('',#4679,#1213);
#983=LINE('',#4681,#1214);
#984=LINE('',#4685,#1215);
#985=LINE('',#4687,#1216);
#986=LINE('',#4689,#1217);
#987=LINE('',#4690,#1218);
#988=LINE('',#4692,#1219);
#989=LINE('',#4693,#1220);
#990=LINE('',#4695,#1221);
#991=LINE('',#4697,#1222);
#992=LINE('',#4701,#1223);
#993=LINE('',#4703,#1224);
#994=LINE('',#4704,#1225);
#995=LINE('',#4707,#1226);
#996=LINE('',#4708,#1227);
#997=LINE('',#4711,#1228);
#998=LINE('',#4712,#1229);
#999=LINE('',#4714,#1230);
#1000=LINE('',#4725,#1231);
#1001=LINE('',#4735,#1232);
#1002=LINE('',#4745,#1233);
#1003=LINE('',#4761,#1234);
#1004=LINE('',#4769,#1235);
#1005=LINE('',#4775,#1236);
#1006=LINE('',#4790,#1237);
#1007=LINE('',#4796,#1238);
#1008=LINE('',#4802,#1239);
#1009=LINE('',#4808,#1240);
#1010=LINE('',#4818,#1241);
#1011=LINE('',#4846,#1242);
#1012=LINE('',#4850,#1243);
#1013=LINE('',#4854,#1244);
#1014=LINE('',#4859,#1245);
#1015=LINE('',#4861,#1246);
#1016=LINE('',#4863,#1247);
#1017=LINE('',#4865,#1248);
#1018=LINE('',#4867,#1249);
#1019=LINE('',#4868,#1250);
#1020=LINE('',#4873,#1251);
#1021=LINE('',#4874,#1252);
#1022=LINE('',#4876,#1253);
#1023=LINE('',#4877,#1254);
#1024=LINE('',#4879,#1255);
#1025=LINE('',#4881,#1256);
#1026=LINE('',#4882,#1257);
#1027=LINE('',#4884,#1258);
#1028=LINE('',#4886,#1259);
#1029=LINE('',#4887,#1260);
#1030=LINE('',#4889,#1261);
#1031=LINE('',#4891,#1262);
#1032=LINE('',#4892,#1263);
#1033=LINE('',#4894,#1264);
#1034=LINE('',#4896,#1265);
#1035=LINE('',#4897,#1266);
#1036=LINE('',#4899,#1267);
#1037=LINE('',#4900,#1268);
#1038=LINE('',#4912,#1269);
#1039=LINE('',#4920,#1270);
#1040=LINE('',#4926,#1271);
#1041=LINE('',#4933,#1272);
#1042=LINE('',#5109,#1273);
#1043=LINE('',#5113,#1274);
#1044=LINE('',#5144,#1275);
#1045=LINE('',#5155,#1276);
#1046=LINE('',#5194,#1277);
#1047=LINE('',#5233,#1278);
#1048=LINE('',#5272,#1279);
#1049=VECTOR('',#3377,1000.);
#1050=VECTOR('',#3380,1000.);
#1051=VECTOR('',#3385,1000.);
#1052=VECTOR('',#3388,1000.);
#1053=VECTOR('',#3393,2.64999999999999);
#1054=VECTOR('',#3400,2.64999999999999);
#1055=VECTOR('',#3407,2.64999999999999);
#1056=VECTOR('',#3414,2.64999999999999);
#1057=VECTOR('',#3421,2.64999999999999);
#1058=VECTOR('',#3428,2.64999999999999);
#1059=VECTOR('',#3435,2.64999999999999);
#1060=VECTOR('',#3442,2.64999999999999);
#1061=VECTOR('',#3449,2.64999999999999);
#1062=VECTOR('',#3456,2.64999999999999);
#1063=VECTOR('',#3461,1000.);
#1064=VECTOR('',#3462,1000.);
#1065=VECTOR('',#3463,1000.);
#1066=VECTOR('',#3464,1000.);
#1067=VECTOR('',#3467,1000.);
#1068=VECTOR('',#3468,1000.);
#1069=VECTOR('',#3469,1000.);
#1070=VECTOR('',#3470,1000.);
#1071=VECTOR('',#3473,1000.);
#1072=VECTOR('',#3474,1000.);
#1073=VECTOR('',#3475,1000.);
#1074=VECTOR('',#3476,1000.);
#1075=VECTOR('',#3479,1000.);
#1076=VECTOR('',#3480,1000.);
#1077=VECTOR('',#3481,1000.);
#1078=VECTOR('',#3482,1000.);
#1079=VECTOR('',#3483,1000.);
#1080=VECTOR('',#3484,1000.);
#1081=VECTOR('',#3485,1000.);
#1082=VECTOR('',#3486,1000.);
#1083=VECTOR('',#3487,1000.);
#1084=VECTOR('',#3490,1000.);
#1085=VECTOR('',#3491,1000.);
#1086=VECTOR('',#3492,1000.);
#1087=VECTOR('',#3495,1000.);
#1088=VECTOR('',#3496,1000.);
#1089=VECTOR('',#3497,1000.);
#1090=VECTOR('',#3498,1000.);
#1091=VECTOR('',#3499,1000.);
#1092=VECTOR('',#3500,1000.);
#1093=VECTOR('',#3501,1000.);
#1094=VECTOR('',#3502,1000.);
#1095=VECTOR('',#3509,1000.);
#1096=VECTOR('',#3510,1000.);
#1097=VECTOR('',#3513,1000.);
#1098=VECTOR('',#3516,1000.);
#1099=VECTOR('',#3519,1000.);
#1100=VECTOR('',#3520,1000.);
#1101=VECTOR('',#3525,1000.);
#1102=VECTOR('',#3526,1000.);
#1103=VECTOR('',#3529,1000.);
#1104=VECTOR('',#3532,1000.);
#1105=VECTOR('',#3535,1000.);
#1106=VECTOR('',#3536,1000.);
#1107=VECTOR('',#3541,1000.);
#1108=VECTOR('',#3544,1000.);
#1109=VECTOR('',#3549,1000.);
#1110=VECTOR('',#3550,1000.);
#1111=VECTOR('',#3561,2.64999999999999);
#1112=VECTOR('',#3568,2.64999999999999);
#1113=VECTOR('',#3575,2.64999999999999);
#1114=VECTOR('',#3582,2.64999999999999);
#1115=VECTOR('',#3589,2.64999999999999);
#1116=VECTOR('',#3594,1000.);
#1117=VECTOR('',#3595,1000.);
#1118=VECTOR('',#3596,1000.);
#1119=VECTOR('',#3597,1000.);
#1120=VECTOR('',#3600,1000.);
#1121=VECTOR('',#3601,1000.);
#1122=VECTOR('',#3602,1000.);
#1123=VECTOR('',#3605,1000.);
#1124=VECTOR('',#3606,1000.);
#1125=VECTOR('',#3607,1000.);
#1126=VECTOR('',#3610,1000.);
#1127=VECTOR('',#3611,1000.);
#1128=VECTOR('',#3614,1000.);
#1129=VECTOR('',#3615,1000.);
#1130=VECTOR('',#3616,1000.);
#1131=VECTOR('',#3617,1000.);
#1132=VECTOR('',#3620,1000.);
#1133=VECTOR('',#3621,1000.);
#1134=VECTOR('',#3622,1000.);
#1135=VECTOR('',#3625,1000.);
#1136=VECTOR('',#3626,1000.);
#1137=VECTOR('',#3627,1000.);
#1138=VECTOR('',#3630,1000.);
#1139=VECTOR('',#3631,1000.);
#1140=VECTOR('',#3634,1000.);
#1141=VECTOR('',#3635,1000.);
#1142=VECTOR('',#3636,1000.);
#1143=VECTOR('',#3637,1000.);
#1144=VECTOR('',#3640,1000.);
#1145=VECTOR('',#3641,1000.);
#1146=VECTOR('',#3642,1000.);
#1147=VECTOR('',#3645,1000.);
#1148=VECTOR('',#3646,1000.);
#1149=VECTOR('',#3647,1000.);
#1150=VECTOR('',#3650,1000.);
#1151=VECTOR('',#3651,1000.);
#1152=VECTOR('',#3654,1000.);
#1153=VECTOR('',#3655,1000.);
#1154=VECTOR('',#3656,1000.);
#1155=VECTOR('',#3657,1000.);
#1156=VECTOR('',#3660,1000.);
#1157=VECTOR('',#3661,1000.);
#1158=VECTOR('',#3662,1000.);
#1159=VECTOR('',#3665,1000.);
#1160=VECTOR('',#3666,1000.);
#1161=VECTOR('',#3667,1000.);
#1162=VECTOR('',#3670,1000.);
#1163=VECTOR('',#3671,1000.);
#1164=VECTOR('',#3674,1000.);
#1165=VECTOR('',#3675,1000.);
#1166=VECTOR('',#3676,1000.);
#1167=VECTOR('',#3677,1000.);
#1168=VECTOR('',#3678,1000.);
#1169=VECTOR('',#3679,1000.);
#1170=VECTOR('',#3682,1000.);
#1171=VECTOR('',#3683,1000.);
#1172=VECTOR('',#3684,1000.);
#1173=VECTOR('',#3685,1000.);
#1174=VECTOR('',#3686,1000.);
#1175=VECTOR('',#3687,1000.);
#1176=VECTOR('',#3690,1000.);
#1177=VECTOR('',#3691,1000.);
#1178=VECTOR('',#3694,1000.);
#1179=VECTOR('',#3695,1000.);
#1180=VECTOR('',#3696,1000.);
#1181=VECTOR('',#3697,1000.);
#1182=VECTOR('',#3698,1000.);
#1183=VECTOR('',#3699,1000.);
#1184=VECTOR('',#3700,1000.);
#1185=VECTOR('',#3701,1000.);
#1186=VECTOR('',#3702,1000.);
#1187=VECTOR('',#3705,1000.);
#1188=VECTOR('',#3706,1000.);
#1189=VECTOR('',#3707,1000.);
#1190=VECTOR('',#3708,1000.);
#1191=VECTOR('',#3709,1000.);
#1192=VECTOR('',#3710,1000.);
#1193=VECTOR('',#3711,1000.);
#1194=VECTOR('',#3712,1000.);
#1195=VECTOR('',#3713,1000.);
#1196=VECTOR('',#3716,1000.);
#1197=VECTOR('',#3717,1000.);
#1198=VECTOR('',#3724,1000.);
#1199=VECTOR('',#3725,1000.);
#1200=VECTOR('',#3728,1000.);
#1201=VECTOR('',#3731,1000.);
#1202=VECTOR('',#3736,1000.);
#1203=VECTOR('',#3737,1000.);
#1204=VECTOR('',#3740,1000.);
#1205=VECTOR('',#3743,1000.);
#1206=VECTOR('',#3756,10.);
#1207=VECTOR('',#3773,1000.);
#1208=VECTOR('',#3776,1000.);
#1209=VECTOR('',#3779,1000.);
#1210=VECTOR('',#3782,1000.);
#1211=VECTOR('',#3785,1000.);
#1212=VECTOR('',#3788,1000.);
#1213=VECTOR('',#3791,1000.);
#1214=VECTOR('',#3794,1000.);
#1215=VECTOR('',#3797,1000.);
#1216=VECTOR('',#3798,1000.);
#1217=VECTOR('',#3799,1000.);
#1218=VECTOR('',#3800,1000.);
#1219=VECTOR('',#3803,1000.);
#1220=VECTOR('',#3804,1000.);
#1221=VECTOR('',#3807,1000.);
#1222=VECTOR('',#3810,1000.);
#1223=VECTOR('',#3815,1000.);
#1224=VECTOR('',#3816,1000.);
#1225=VECTOR('',#3817,1000.);
#1226=VECTOR('',#3820,1000.);
#1227=VECTOR('',#3821,1000.);
#1228=VECTOR('',#3824,1000.);
#1229=VECTOR('',#3825,1000.);
#1230=VECTOR('',#3828,1000.);
#1231=VECTOR('',#3843,13.5);
#1232=VECTOR('',#3856,12.775);
#1233=VECTOR('',#3867,12.45);
#1234=VECTOR('',#3888,10.);
#1235=VECTOR('',#3899,11.05);
#1236=VECTOR('',#3906,10.725);
#1237=VECTOR('',#3929,13.5);
#1238=VECTOR('',#3936,13.5);
#1239=VECTOR('',#3943,22.5);
#1240=VECTOR('',#3950,10.5);
#1241=VECTOR('',#3965,2.042);
#1242=VECTOR('',#3998,4.25);
#1243=VECTOR('',#4003,2.5);
#1244=VECTOR('',#4008,2.055);
#1245=VECTOR('',#4013,1000.);
#1246=VECTOR('',#4014,1000.);
#1247=VECTOR('',#4015,1000.);
#1248=VECTOR('',#4016,1000.);
#1249=VECTOR('',#4017,1000.);
#1250=VECTOR('',#4018,1000.);
#1251=VECTOR('',#4025,1000.);
#1252=VECTOR('',#4026,1000.);
#1253=VECTOR('',#4027,1000.);
#1254=VECTOR('',#4028,1000.);
#1255=VECTOR('',#4031,1000.);
#1256=VECTOR('',#4032,1000.);
#1257=VECTOR('',#4033,1000.);
#1258=VECTOR('',#4036,1000.);
#1259=VECTOR('',#4037,1000.);
#1260=VECTOR('',#4038,1000.);
#1261=VECTOR('',#4041,1000.);
#1262=VECTOR('',#4042,1000.);
#1263=VECTOR('',#4043,1000.);
#1264=VECTOR('',#4046,1000.);
#1265=VECTOR('',#4047,1000.);
#1266=VECTOR('',#4048,1000.);
#1267=VECTOR('',#4051,1000.);
#1268=VECTOR('',#4052,1000.);
#1269=VECTOR('',#4071,2.5);
#1270=VECTOR('',#4080,2.5);
#1271=VECTOR('',#4087,2.06);
#1272=VECTOR('',#4094,5.56078137864557);
#1273=VECTOR('',#4105,2.1);
#1274=VECTOR('',#4108,1000.);
#1275=VECTOR('',#4109,1000.);
#1276=VECTOR('',#4112,1000.);
#1277=VECTOR('',#4115,1000.);
#1278=VECTOR('',#4118,1000.);
#1279=VECTOR('',#4121,1000.);
#1280=CIRCLE('',#3049,60.);
#1281=CIRCLE('',#3050,60.);
#1282=CIRCLE('',#3052,60.);
#1283=CIRCLE('',#3053,60.);
#1284=CIRCLE('',#3055,2.64999999999999);
#1285=CIRCLE('',#3056,2.64999999999999);
#1286=CIRCLE('',#3058,2.64999999999999);
#1287=CIRCLE('',#3059,2.64999999999999);
#1288=CIRCLE('',#3061,2.64999999999999);
#1289=CIRCLE('',#3062,2.64999999999999);
#1290=CIRCLE('',#3064,2.64999999999999);
#1291=CIRCLE('',#3065,2.64999999999999);
#1292=CIRCLE('',#3067,2.64999999999999);
#1293=CIRCLE('',#3068,2.64999999999999);
#1294=CIRCLE('',#3070,2.64999999999999);
#1295=CIRCLE('',#3071,2.64999999999999);
#1296=CIRCLE('',#3073,2.64999999999999);
#1297=CIRCLE('',#3074,2.64999999999999);
#1298=CIRCLE('',#3076,2.64999999999999);
#1299=CIRCLE('',#3077,2.64999999999999);
#1300=CIRCLE('',#3079,2.64999999999999);
#1301=CIRCLE('',#3080,2.64999999999999);
#1302=CIRCLE('',#3082,2.64999999999999);
#1303=CIRCLE('',#3083,2.64999999999999);
#1304=CIRCLE('',#3093,60.);
#1305=CIRCLE('',#3095,60.);
#1306=CIRCLE('',#3098,60.);
#1307=CIRCLE('',#3100,60.);
#1308=CIRCLE('',#3110,2.64999999999999);
#1309=CIRCLE('',#3111,2.64999999999999);
#1310=CIRCLE('',#3113,2.64999999999999);
#1311=CIRCLE('',#3114,2.64999999999999);
#1312=CIRCLE('',#3116,2.64999999999999);
#1313=CIRCLE('',#3117,2.64999999999999);
#1314=CIRCLE('',#3119,2.64999999999999);
#1315=CIRCLE('',#3120,2.64999999999999);
#1316=CIRCLE('',#3122,2.64999999999999);
#1317=CIRCLE('',#3123,2.64999999999999);
#1318=CIRCLE('',#3158,10.);
#1319=CIRCLE('',#3159,10.);
#1320=CIRCLE('',#3160,10.);
#1321=CIRCLE('',#3161,10.);
#1322=CIRCLE('',#3162,10.);
#1323=CIRCLE('',#3163,10.);
#1324=CIRCLE('',#3164,10.);
#1325=CIRCLE('',#3165,10.);
#1326=CIRCLE('',#3166,10.);
#1327=CIRCLE('',#3167,10.);
#1328=CIRCLE('',#3188,13.3);
#1329=CIRCLE('',#3189,0.200000000000003);
#1330=CIRCLE('',#3190,13.5);
#1331=CIRCLE('',#3192,13.5);
#1332=CIRCLE('',#3194,0.200000000000003);
#1333=CIRCLE('',#3195,13.3);
#1334=CIRCLE('',#3197,12.775);
#1335=CIRCLE('',#3198,12.775);
#1336=CIRCLE('',#3199,12.775);
#1337=CIRCLE('',#3201,12.45);
#1338=CIRCLE('',#3202,12.45);
#1339=CIRCLE('',#3203,12.45);
#1340=CIRCLE('',#3205,11.05);
#1341=CIRCLE('',#3206,1.05);
#1342=CIRCLE('',#3207,11.05);
#1343=CIRCLE('',#3209,10.2);
#1344=CIRCLE('',#3210,0.200000000000003);
#1345=CIRCLE('',#3211,10.);
#1346=CIRCLE('',#3213,10.);
#1347=CIRCLE('',#3215,0.200000000000003);
#1348=CIRCLE('',#3216,10.2);
#1349=CIRCLE('',#3218,11.05);
#1350=CIRCLE('',#3220,10.725);
#1351=CIRCLE('',#3221,10.725);
#1352=CIRCLE('',#3222,10.725);
#1353=CIRCLE('',#3224,1.05);
#1354=CIRCLE('',#3231,13.5);
#1355=CIRCLE('',#3232,13.5);
#1356=CIRCLE('',#3234,13.5);
#1357=CIRCLE('',#3235,13.5);
#1358=CIRCLE('',#3237,22.5);
#1359=CIRCLE('',#3238,22.5);
#1360=CIRCLE('',#3240,10.5);
#1361=CIRCLE('',#3241,10.5);
#1362=CIRCLE('',#3248,2.042);
#1363=CIRCLE('',#3249,2.042);
#1364=CIRCLE('',#3250,2.042);
#1365=CIRCLE('',#3251,2.042);
#1366=CIRCLE('',#3252,2.042);
#1367=CIRCLE('',#3253,2.042);
#1368=CIRCLE('',#3255,4.);
#1369=CIRCLE('',#3256,0.25);
#1370=CIRCLE('',#3257,4.25);
#1371=CIRCLE('',#3259,2.5);
#1372=CIRCLE('',#3260,2.5);
#1373=CIRCLE('',#3261,0.2);
#1374=CIRCLE('',#3262,2.7);
#1375=CIRCLE('',#3264,4.25);
#1376=CIRCLE('',#3266,2.5);
#1377=CIRCLE('',#3268,2.055);
#1378=CIRCLE('',#3286,2.5);
#1379=CIRCLE('',#3287,2.5);
#1380=CIRCLE('',#3288,2.5);
#1381=CIRCLE('',#3290,2.1);
#1382=CIRCLE('',#3291,2.1);
#1383=CIRCLE('',#3293,2.1);
#1384=CIRCLE('',#3294,2.5);
#1385=CIRCLE('',#3296,5.56078137864557);
#1386=CIRCLE('',#3297,5.56078137864557);
#1387=CIRCLE('',#3299,0.51554560206288);
#1388=CIRCLE('',#3300,5.38445439793712);
#1389=CIRCLE('',#3309,4.);
#1390=CIRCLE('',#3310,4.);
#1391=CIRCLE('',#3311,4.);
#1392=CIRCLE('',#3312,4.);
#1393=CIRCLE('',#3313,4.);
#1394=CIRCLE('',#3314,4.);
#1395=VERTEX_POINT('',#4249);
#1396=VERTEX_POINT('',#4250);
#1397=VERTEX_POINT('',#4252);
#1398=VERTEX_POINT('',#4254);
#1399=VERTEX_POINT('',#4258);
#1400=VERTEX_POINT('',#4259);
#1401=VERTEX_POINT('',#4261);
#1402=VERTEX_POINT('',#4263);
#1403=VERTEX_POINT('',#4267);
#1404=VERTEX_POINT('',#4269);
#1405=VERTEX_POINT('',#4273);
#1406=VERTEX_POINT('',#4275);
#1407=VERTEX_POINT('',#4279);
#1408=VERTEX_POINT('',#4281);
#1409=VERTEX_POINT('',#4285);
#1410=VERTEX_POINT('',#4287);
#1411=VERTEX_POINT('',#4291);
#1412=VERTEX_POINT('',#4293);
#1413=VERTEX_POINT('',#4297);
#1414=VERTEX_POINT('',#4299);
#1415=VERTEX_POINT('',#4303);
#1416=VERTEX_POINT('',#4305);
#1417=VERTEX_POINT('',#4309);
#1418=VERTEX_POINT('',#4311);
#1419=VERTEX_POINT('',#4315);
#1420=VERTEX_POINT('',#4317);
#1421=VERTEX_POINT('',#4321);
#1422=VERTEX_POINT('',#4323);
#1423=VERTEX_POINT('',#4327);
#1424=VERTEX_POINT('',#4328);
#1425=VERTEX_POINT('',#4330);
#1426=VERTEX_POINT('',#4332);
#1427=VERTEX_POINT('',#4336);
#1428=VERTEX_POINT('',#4337);
#1429=VERTEX_POINT('',#4339);
#1430=VERTEX_POINT('',#4341);
#1431=VERTEX_POINT('',#4345);
#1432=VERTEX_POINT('',#4346);
#1433=VERTEX_POINT('',#4348);
#1434=VERTEX_POINT('',#4350);
#1435=VERTEX_POINT('',#4354);
#1436=VERTEX_POINT('',#4356);
#1437=VERTEX_POINT('',#4359);
#1438=VERTEX_POINT('',#4361);
#1439=VERTEX_POINT('',#4364);
#1440=VERTEX_POINT('',#4366);
#1441=VERTEX_POINT('',#4370);
#1442=VERTEX_POINT('',#4372);
#1443=VERTEX_POINT('',#4377);
#1444=VERTEX_POINT('',#4379);
#1445=VERTEX_POINT('',#4382);
#1446=VERTEX_POINT('',#4384);
#1447=VERTEX_POINT('',#4392);
#1448=VERTEX_POINT('',#4394);
#1449=VERTEX_POINT('',#4399);
#1450=VERTEX_POINT('',#4400);
#1451=VERTEX_POINT('',#4407);
#1452=VERTEX_POINT('',#4409);
#1453=VERTEX_POINT('',#4414);
#1454=VERTEX_POINT('',#4415);
#1455=VERTEX_POINT('',#4432);
#1456=VERTEX_POINT('',#4434);
#1457=VERTEX_POINT('',#4438);
#1458=VERTEX_POINT('',#4440);
#1459=VERTEX_POINT('',#4444);
#1460=VERTEX_POINT('',#4446);
#1461=VERTEX_POINT('',#4450);
#1462=VERTEX_POINT('',#4452);
#1463=VERTEX_POINT('',#4456);
#1464=VERTEX_POINT('',#4458);
#1465=VERTEX_POINT('',#4462);
#1466=VERTEX_POINT('',#4463);
#1467=VERTEX_POINT('',#4465);
#1468=VERTEX_POINT('',#4467);
#1469=VERTEX_POINT('',#4471);
#1470=VERTEX_POINT('',#4473);
#1471=VERTEX_POINT('',#4477);
#1472=VERTEX_POINT('',#4479);
#1473=VERTEX_POINT('',#4486);
#1474=VERTEX_POINT('',#4487);
#1475=VERTEX_POINT('',#4489);
#1476=VERTEX_POINT('',#4491);
#1477=VERTEX_POINT('',#4495);
#1478=VERTEX_POINT('',#4497);
#1479=VERTEX_POINT('',#4501);
#1480=VERTEX_POINT('',#4503);
#1481=VERTEX_POINT('',#4510);
#1482=VERTEX_POINT('',#4511);
#1483=VERTEX_POINT('',#4513);
#1484=VERTEX_POINT('',#4515);
#1485=VERTEX_POINT('',#4519);
#1486=VERTEX_POINT('',#4521);
#1487=VERTEX_POINT('',#4525);
#1488=VERTEX_POINT('',#4527);
#1489=VERTEX_POINT('',#4534);
#1490=VERTEX_POINT('',#4535);
#1491=VERTEX_POINT('',#4537);
#1492=VERTEX_POINT('',#4539);
#1493=VERTEX_POINT('',#4543);
#1494=VERTEX_POINT('',#4545);
#1495=VERTEX_POINT('',#4549);
#1496=VERTEX_POINT('',#4551);
#1497=VERTEX_POINT('',#4558);
#1498=VERTEX_POINT('',#4559);
#1499=VERTEX_POINT('',#4561);
#1500=VERTEX_POINT('',#4563);
#1501=VERTEX_POINT('',#4565);
#1502=VERTEX_POINT('',#4567);
#1503=VERTEX_POINT('',#4571);
#1504=VERTEX_POINT('',#4572);
#1505=VERTEX_POINT('',#4574);
#1506=VERTEX_POINT('',#4576);
#1507=VERTEX_POINT('',#4578);
#1508=VERTEX_POINT('',#4580);
#1509=VERTEX_POINT('',#4588);
#1510=VERTEX_POINT('',#4589);
#1511=VERTEX_POINT('',#4591);
#1512=VERTEX_POINT('',#4593);
#1513=VERTEX_POINT('',#4596);
#1514=VERTEX_POINT('',#4597);
#1515=VERTEX_POINT('',#4599);
#1516=VERTEX_POINT('',#4601);
#1517=VERTEX_POINT('',#4606);
#1518=VERTEX_POINT('',#4607);
#1519=VERTEX_POINT('',#4609);
#1520=VERTEX_POINT('',#4611);
#1521=VERTEX_POINT('',#4614);
#1522=VERTEX_POINT('',#4615);
#1523=VERTEX_POINT('',#4617);
#1524=VERTEX_POINT('',#4619);
#1525=VERTEX_POINT('',#4645);
#1526=VERTEX_POINT('',#4646);
#1527=VERTEX_POINT('',#4648);
#1528=VERTEX_POINT('',#4650);
#1529=VERTEX_POINT('',#4652);
#1530=VERTEX_POINT('',#4654);
#1531=VERTEX_POINT('',#4656);
#1532=VERTEX_POINT('',#4658);
#1533=VERTEX_POINT('',#4660);
#1534=VERTEX_POINT('',#4663);
#1535=VERTEX_POINT('',#4683);
#1536=VERTEX_POINT('',#4684);
#1537=VERTEX_POINT('',#4686);
#1538=VERTEX_POINT('',#4688);
#1539=VERTEX_POINT('',#4700);
#1540=VERTEX_POINT('',#4702);
#1541=VERTEX_POINT('',#4706);
#1542=VERTEX_POINT('',#4710);
#1543=VERTEX_POINT('',#4718);
#1544=VERTEX_POINT('',#4720);
#1545=VERTEX_POINT('',#4724);
#1546=VERTEX_POINT('',#4728);
#1547=VERTEX_POINT('',#4732);
#1548=VERTEX_POINT('',#4734);
#1549=VERTEX_POINT('',#4736);
#1550=VERTEX_POINT('',#4740);
#1551=VERTEX_POINT('',#4741);
#1552=VERTEX_POINT('',#4744);
#1553=VERTEX_POINT('',#4748);
#1554=VERTEX_POINT('',#4749);
#1555=VERTEX_POINT('',#4754);
#1556=VERTEX_POINT('',#4756);
#1557=VERTEX_POINT('',#4760);
#1558=VERTEX_POINT('',#4764);
#1559=VERTEX_POINT('',#4768);
#1560=VERTEX_POINT('',#4772);
#1561=VERTEX_POINT('',#4774);
#1562=VERTEX_POINT('',#4776);
#1563=VERTEX_POINT('',#4787);
#1564=VERTEX_POINT('',#4789);
#1565=VERTEX_POINT('',#4793);
#1566=VERTEX_POINT('',#4795);
#1567=VERTEX_POINT('',#4799);
#1568=VERTEX_POINT('',#4801);
#1569=VERTEX_POINT('',#4805);
#1570=VERTEX_POINT('',#4807);
#1571=VERTEX_POINT('',#4816);
#1572=VERTEX_POINT('',#4817);
#1573=VERTEX_POINT('',#4819);
#1574=VERTEX_POINT('',#4821);
#1575=VERTEX_POINT('',#4823);
#1576=VERTEX_POINT('',#4825);
#1577=VERTEX_POINT('',#4827);
#1578=VERTEX_POINT('',#4831);
#1579=VERTEX_POINT('',#4833);
#1580=VERTEX_POINT('',#4837);
#1581=VERTEX_POINT('',#4838);
#1582=VERTEX_POINT('',#4841);
#1583=VERTEX_POINT('',#4845);
#1584=VERTEX_POINT('',#4849);
#1585=VERTEX_POINT('',#4853);
#1586=VERTEX_POINT('',#4857);
#1587=VERTEX_POINT('',#4858);
#1588=VERTEX_POINT('',#4860);
#1589=VERTEX_POINT('',#4862);
#1590=VERTEX_POINT('',#4864);
#1591=VERTEX_POINT('',#4866);
#1592=VERTEX_POINT('',#4872);
#1593=VERTEX_POINT('',#4875);
#1594=VERTEX_POINT('',#4880);
#1595=VERTEX_POINT('',#4885);
#1596=VERTEX_POINT('',#4890);
#1597=VERTEX_POINT('',#4895);
#1598=VERTEX_POINT('',#4909);
#1599=VERTEX_POINT('',#4911);
#1600=VERTEX_POINT('',#4913);
#1601=VERTEX_POINT('',#4917);
#1602=VERTEX_POINT('',#4918);
#1603=VERTEX_POINT('',#4923);
#1604=VERTEX_POINT('',#4925);
#1605=VERTEX_POINT('',#4929);
#1606=VERTEX_POINT('',#4930);
#1607=VERTEX_POINT('',#4932);
#1608=VERTEX_POINT('',#4934);
#1609=VERTEX_POINT('',#4941);
#1610=VERTEX_POINT('',#4973);
#1611=VERTEX_POINT('',#5005);
#1612=VERTEX_POINT('',#5019);
#1613=VERTEX_POINT('',#5026);
#1614=VERTEX_POINT('',#5058);
#1615=VERTEX_POINT('',#5105);
#1616=VERTEX_POINT('',#5111);
#1617=VERTEX_POINT('',#5112);
#1618=VERTEX_POINT('',#5114);
#1619=VERTEX_POINT('',#5143);
#1620=VERTEX_POINT('',#5145);
#1621=VERTEX_POINT('',#5153);
#1622=VERTEX_POINT('',#5154);
#1623=VERTEX_POINT('',#5184);
#1624=VERTEX_POINT('',#5192);
#1625=VERTEX_POINT('',#5193);
#1626=VERTEX_POINT('',#5223);
#1627=VERTEX_POINT('',#5231);
#1628=VERTEX_POINT('',#5232);
#1629=VERTEX_POINT('',#5262);
#1630=VERTEX_POINT('',#5270);
#1631=VERTEX_POINT('',#5271);
#1632=VERTEX_POINT('',#5301);
#1633=VERTEX_POINT('',#5337);
#1634=EDGE_CURVE('',#1395,#1396,#1280,.T.);
#1635=EDGE_CURVE('',#1395,#1397,#818,.T.);
#1636=EDGE_CURVE('',#1397,#1398,#1281,.T.);
#1637=EDGE_CURVE('',#1396,#1398,#819,.T.);
#1638=EDGE_CURVE('',#1399,#1400,#1282,.T.);
#1639=EDGE_CURVE('',#1399,#1401,#820,.T.);
#1640=EDGE_CURVE('',#1401,#1402,#1283,.T.);
#1641=EDGE_CURVE('',#1400,#1402,#821,.T.);
#1642=EDGE_CURVE('',#1403,#1403,#1284,.T.);
#1643=EDGE_CURVE('',#1403,#1404,#822,.T.);
#1644=EDGE_CURVE('',#1404,#1404,#1285,.T.);
#1645=EDGE_CURVE('',#1405,#1405,#1286,.T.);
#1646=EDGE_CURVE('',#1405,#1406,#823,.T.);
#1647=EDGE_CURVE('',#1406,#1406,#1287,.T.);
#1648=EDGE_CURVE('',#1407,#1407,#1288,.T.);
#1649=EDGE_CURVE('',#1407,#1408,#824,.T.);
#1650=EDGE_CURVE('',#1408,#1408,#1289,.T.);
#1651=EDGE_CURVE('',#1409,#1409,#1290,.T.);
#1652=EDGE_CURVE('',#1409,#1410,#825,.T.);
#1653=EDGE_CURVE('',#1410,#1410,#1291,.T.);
#1654=EDGE_CURVE('',#1411,#1411,#1292,.T.);
#1655=EDGE_CURVE('',#1411,#1412,#826,.T.);
#1656=EDGE_CURVE('',#1412,#1412,#1293,.T.);
#1657=EDGE_CURVE('',#1413,#1413,#1294,.T.);
#1658=EDGE_CURVE('',#1413,#1414,#827,.T.);
#1659=EDGE_CURVE('',#1414,#1414,#1295,.T.);
#1660=EDGE_CURVE('',#1415,#1415,#1296,.T.);
#1661=EDGE_CURVE('',#1415,#1416,#828,.T.);
#1662=EDGE_CURVE('',#1416,#1416,#1297,.T.);
#1663=EDGE_CURVE('',#1417,#1417,#1298,.T.);
#1664=EDGE_CURVE('',#1417,#1418,#829,.T.);
#1665=EDGE_CURVE('',#1418,#1418,#1299,.T.);
#1666=EDGE_CURVE('',#1419,#1419,#1300,.T.);
#1667=EDGE_CURVE('',#1419,#1420,#830,.T.);
#1668=EDGE_CURVE('',#1420,#1420,#1301,.T.);
#1669=EDGE_CURVE('',#1421,#1421,#1302,.T.);
#1670=EDGE_CURVE('',#1421,#1422,#831,.T.);
#1671=EDGE_CURVE('',#1422,#1422,#1303,.T.);
#1672=EDGE_CURVE('',#1423,#1424,#832,.T.);
#1673=EDGE_CURVE('',#1423,#1425,#833,.T.);
#1674=EDGE_CURVE('',#1425,#1426,#834,.T.);
#1675=EDGE_CURVE('',#1424,#1426,#835,.T.);
#1676=EDGE_CURVE('',#1427,#1428,#836,.T.);
#1677=EDGE_CURVE('',#1427,#1429,#837,.T.);
#1678=EDGE_CURVE('',#1429,#1430,#838,.T.);
#1679=EDGE_CURVE('',#1428,#1430,#839,.T.);
#1680=EDGE_CURVE('',#1431,#1432,#840,.T.);
#1681=EDGE_CURVE('',#1432,#1433,#841,.T.);
#1682=EDGE_CURVE('',#1434,#1433,#842,.T.);
#1683=EDGE_CURVE('',#1431,#1434,#843,.T.);
#1684=EDGE_CURVE('',#1435,#1430,#844,.T.);
#1685=EDGE_CURVE('',#1436,#1435,#845,.T.);
#1686=EDGE_CURVE('',#1436,#1434,#846,.T.);
#1687=EDGE_CURVE('',#1437,#1433,#847,.T.);
#1688=EDGE_CURVE('',#1437,#1438,#848,.T.);
#1689=EDGE_CURVE('',#1438,#1424,#849,.T.);
#1690=EDGE_CURVE('',#1439,#1426,#850,.T.);
#1691=EDGE_CURVE('',#1439,#1440,#851,.T.);
#1692=EDGE_CURVE('',#1440,#1428,#852,.T.);
#1693=EDGE_CURVE('',#1441,#1435,#853,.T.);
#1694=EDGE_CURVE('',#1442,#1441,#854,.T.);
#1695=EDGE_CURVE('',#1442,#1436,#855,.T.);
#1696=EDGE_CURVE('',#1429,#1441,#856,.T.);
#1697=EDGE_CURVE('',#1443,#1427,#857,.T.);
#1698=EDGE_CURVE('',#1443,#1444,#858,.T.);
#1699=EDGE_CURVE('',#1444,#1425,#859,.T.);
#1700=EDGE_CURVE('',#1445,#1423,#860,.T.);
#1701=EDGE_CURVE('',#1445,#1446,#861,.T.);
#1702=EDGE_CURVE('',#1446,#1432,#862,.T.);
#1703=EDGE_CURVE('',#1431,#1442,#863,.T.);
#1704=EDGE_CURVE('',#1443,#1440,#864,.T.);
#1705=EDGE_CURVE('',#1396,#1447,#865,.T.);
#1706=EDGE_CURVE('',#1447,#1448,#1304,.T.);
#1707=EDGE_CURVE('',#1448,#1395,#866,.T.);
#1708=EDGE_CURVE('',#1444,#1439,#867,.T.);
#1709=EDGE_CURVE('',#1449,#1450,#1305,.T.);
#1710=EDGE_CURVE('',#1398,#1449,#868,.T.);
#1711=EDGE_CURVE('',#1450,#1397,#869,.T.);
#1712=EDGE_CURVE('',#1445,#1438,#870,.T.);
#1713=EDGE_CURVE('',#1400,#1451,#871,.T.);
#1714=EDGE_CURVE('',#1451,#1452,#1306,.T.);
#1715=EDGE_CURVE('',#1452,#1399,#872,.T.);
#1716=EDGE_CURVE('',#1446,#1437,#873,.T.);
#1717=EDGE_CURVE('',#1453,#1454,#1307,.T.);
#1718=EDGE_CURVE('',#1402,#1453,#874,.T.);
#1719=EDGE_CURVE('',#1454,#1401,#875,.T.);
#1720=EDGE_CURVE('',#1452,#1454,#876,.T.);
#1721=EDGE_CURVE('',#1451,#1453,#877,.T.);
#1722=EDGE_CURVE('',#1447,#1449,#878,.T.);
#1723=EDGE_CURVE('',#1448,#1450,#879,.T.);
#1724=EDGE_CURVE('',#1455,#1455,#1308,.T.);
#1725=EDGE_CURVE('',#1455,#1456,#880,.T.);
#1726=EDGE_CURVE('',#1456,#1456,#1309,.T.);
#1727=EDGE_CURVE('',#1457,#1457,#1310,.T.);
#1728=EDGE_CURVE('',#1457,#1458,#881,.T.);
#1729=EDGE_CURVE('',#1458,#1458,#1311,.T.);
#1730=EDGE_CURVE('',#1459,#1459,#1312,.T.);
#1731=EDGE_CURVE('',#1459,#1460,#882,.T.);
#1732=EDGE_CURVE('',#1460,#1460,#1313,.T.);
#1733=EDGE_CURVE('',#1461,#1461,#1314,.T.);
#1734=EDGE_CURVE('',#1461,#1462,#883,.T.);
#1735=EDGE_CURVE('',#1462,#1462,#1315,.T.);
#1736=EDGE_CURVE('',#1463,#1463,#1316,.T.);
#1737=EDGE_CURVE('',#1463,#1464,#884,.T.);
#1738=EDGE_CURVE('',#1464,#1464,#1317,.T.);
#1739=EDGE_CURVE('',#1465,#1466,#885,.T.);
#1740=EDGE_CURVE('',#1466,#1467,#886,.T.);
#1741=EDGE_CURVE('',#1468,#1467,#887,.T.);
#1742=EDGE_CURVE('',#1465,#1468,#888,.T.);
#1743=EDGE_CURVE('',#1467,#1469,#889,.T.);
#1744=EDGE_CURVE('',#1470,#1469,#890,.T.);
#1745=EDGE_CURVE('',#1468,#1470,#891,.T.);
#1746=EDGE_CURVE('',#1469,#1471,#892,.T.);
#1747=EDGE_CURVE('',#1472,#1471,#893,.T.);
#1748=EDGE_CURVE('',#1470,#1472,#894,.T.);
#1749=EDGE_CURVE('',#1471,#1466,#895,.T.);
#1750=EDGE_CURVE('',#1472,#1465,#896,.T.);
#1751=EDGE_CURVE('',#1473,#1474,#897,.T.);
#1752=EDGE_CURVE('',#1474,#1475,#898,.T.);
#1753=EDGE_CURVE('',#1476,#1475,#899,.T.);
#1754=EDGE_CURVE('',#1473,#1476,#900,.T.);
#1755=EDGE_CURVE('',#1475,#1477,#901,.T.);
#1756=EDGE_CURVE('',#1478,#1477,#902,.T.);
#1757=EDGE_CURVE('',#1476,#1478,#903,.T.);
#1758=EDGE_CURVE('',#1477,#1479,#904,.T.);
#1759=EDGE_CURVE('',#1480,#1479,#905,.T.);
#1760=EDGE_CURVE('',#1478,#1480,#906,.T.);
#1761=EDGE_CURVE('',#1479,#1474,#907,.T.);
#1762=EDGE_CURVE('',#1480,#1473,#908,.T.);
#1763=EDGE_CURVE('',#1481,#1482,#909,.T.);
#1764=EDGE_CURVE('',#1482,#1483,#910,.T.);
#1765=EDGE_CURVE('',#1484,#1483,#911,.T.);
#1766=EDGE_CURVE('',#1481,#1484,#912,.T.);
#1767=EDGE_CURVE('',#1483,#1485,#913,.T.);
#1768=EDGE_CURVE('',#1486,#1485,#914,.T.);
#1769=EDGE_CURVE('',#1484,#1486,#915,.T.);
#1770=EDGE_CURVE('',#1485,#1487,#916,.T.);
#1771=EDGE_CURVE('',#1488,#1487,#917,.T.);
#1772=EDGE_CURVE('',#1486,#1488,#918,.T.);
#1773=EDGE_CURVE('',#1487,#1482,#919,.T.);
#1774=EDGE_CURVE('',#1488,#1481,#920,.T.);
#1775=EDGE_CURVE('',#1489,#1490,#921,.T.);
#1776=EDGE_CURVE('',#1490,#1491,#922,.T.);
#1777=EDGE_CURVE('',#1492,#1491,#923,.T.);
#1778=EDGE_CURVE('',#1489,#1492,#924,.T.);
#1779=EDGE_CURVE('',#1491,#1493,#925,.T.);
#1780=EDGE_CURVE('',#1494,#1493,#926,.T.);
#1781=EDGE_CURVE('',#1492,#1494,#927,.T.);
#1782=EDGE_CURVE('',#1493,#1495,#928,.T.);
#1783=EDGE_CURVE('',#1496,#1495,#929,.T.);
#1784=EDGE_CURVE('',#1494,#1496,#930,.T.);
#1785=EDGE_CURVE('',#1495,#1490,#931,.T.);
#1786=EDGE_CURVE('',#1496,#1489,#932,.T.);
#1787=EDGE_CURVE('',#1497,#1498,#933,.T.);
#1788=EDGE_CURVE('',#1498,#1499,#934,.T.);
#1789=EDGE_CURVE('',#1499,#1500,#935,.T.);
#1790=EDGE_CURVE('',#1501,#1500,#936,.T.);
#1791=EDGE_CURVE('',#1502,#1501,#937,.T.);
#1792=EDGE_CURVE('',#1502,#1497,#938,.T.);
#1793=EDGE_CURVE('',#1503,#1504,#939,.T.);
#1794=EDGE_CURVE('',#1505,#1504,#940,.T.);
#1795=EDGE_CURVE('',#1506,#1505,#941,.T.);
#1796=EDGE_CURVE('',#1507,#1506,#942,.T.);
#1797=EDGE_CURVE('',#1508,#1507,#943,.T.);
#1798=EDGE_CURVE('',#1508,#1503,#944,.T.);
#1799=EDGE_CURVE('',#1504,#1497,#945,.T.);
#1800=EDGE_CURVE('',#1505,#1502,#946,.T.);
#1801=EDGE_CURVE('',#1506,#1501,#947,.T.);
#1802=EDGE_CURVE('',#1509,#1510,#948,.T.);
#1803=EDGE_CURVE('',#1511,#1509,#949,.T.);
#1804=EDGE_CURVE('',#1512,#1511,#950,.T.);
#1805=EDGE_CURVE('',#1510,#1512,#951,.T.);
#1806=EDGE_CURVE('',#1513,#1514,#952,.T.);
#1807=EDGE_CURVE('',#1515,#1513,#953,.T.);
#1808=EDGE_CURVE('',#1516,#1515,#954,.T.);
#1809=EDGE_CURVE('',#1514,#1516,#955,.T.);
#1810=EDGE_CURVE('',#1498,#1503,#956,.T.);
#1811=EDGE_CURVE('',#1517,#1518,#957,.T.);
#1812=EDGE_CURVE('',#1518,#1519,#958,.T.);
#1813=EDGE_CURVE('',#1519,#1520,#959,.T.);
#1814=EDGE_CURVE('',#1520,#1517,#960,.T.);
#1815=EDGE_CURVE('',#1521,#1522,#961,.T.);
#1816=EDGE_CURVE('',#1522,#1523,#962,.T.);
#1817=EDGE_CURVE('',#1523,#1524,#963,.T.);
#1818=EDGE_CURVE('',#1524,#1521,#964,.T.);
#1819=EDGE_CURVE('',#1500,#1507,#965,.T.);
#1820=EDGE_CURVE('',#1499,#1508,#966,.T.);
#1821=EDGE_CURVE('',#1521,#1515,#967,.T.);
#1822=EDGE_CURVE('',#1522,#1513,#968,.T.);
#1823=EDGE_CURVE('',#1524,#1516,#969,.T.);
#1824=EDGE_CURVE('',#1523,#1514,#970,.T.);
#1825=EDGE_CURVE('',#1517,#1511,#971,.T.);
#1826=EDGE_CURVE('',#1518,#1509,#972,.T.);
#1827=EDGE_CURVE('',#1520,#1512,#973,.T.);
#1828=EDGE_CURVE('',#1519,#1510,#974,.T.);
#1829=EDGE_CURVE('',#1525,#1526,#1318,.T.);
#1830=EDGE_CURVE('',#1526,#1527,#1319,.T.);
#1831=EDGE_CURVE('',#1527,#1528,#1320,.T.);
#1832=EDGE_CURVE('',#1528,#1529,#975,.T.);
#1833=EDGE_CURVE('',#1530,#1529,#1321,.T.);
#1834=EDGE_CURVE('',#1531,#1530,#1322,.T.);
#1835=EDGE_CURVE('',#1532,#1531,#1323,.T.);
#1836=EDGE_CURVE('',#1533,#1532,#1324,.T.);
#1837=EDGE_CURVE('',#1529,#1533,#1325,.T.);
#1838=EDGE_CURVE('',#1528,#1534,#1326,.T.);
#1839=EDGE_CURVE('',#1534,#1525,#1327,.T.);
#1840=EDGE_CURVE('',#1533,#1530,#976,.T.);
#1841=EDGE_CURVE('',#1532,#1533,#977,.T.);
#1842=EDGE_CURVE('',#1531,#1532,#978,.T.);
#1843=EDGE_CURVE('',#1530,#1531,#979,.T.);
#1844=EDGE_CURVE('',#1534,#1527,#980,.T.);
#1845=EDGE_CURVE('',#1525,#1534,#981,.T.);
#1846=EDGE_CURVE('',#1526,#1525,#982,.T.);
#1847=EDGE_CURVE('',#1527,#1526,#983,.T.);
#1848=EDGE_CURVE('',#1535,#1536,#984,.T.);
#1849=EDGE_CURVE('',#1537,#1535,#985,.T.);
#1850=EDGE_CURVE('',#1538,#1537,#986,.T.);
#1851=EDGE_CURVE('',#1536,#1538,#987,.T.);
#1852=EDGE_CURVE('',#1527,#1535,#988,.T.);
#1853=EDGE_CURVE('',#1526,#1537,#989,.T.);
#1854=EDGE_CURVE('',#1525,#1538,#990,.T.);
#1855=EDGE_CURVE('',#1534,#1536,#991,.T.);
#1856=EDGE_CURVE('',#1539,#1533,#992,.T.);
#1857=EDGE_CURVE('',#1540,#1539,#993,.T.);
#1858=EDGE_CURVE('',#1540,#1530,#994,.T.);
#1859=EDGE_CURVE('',#1541,#1532,#995,.T.);
#1860=EDGE_CURVE('',#1539,#1541,#996,.T.);
#1861=EDGE_CURVE('',#1542,#1531,#997,.T.);
#1862=EDGE_CURVE('',#1541,#1542,#998,.T.);
#1863=EDGE_CURVE('',#1542,#1540,#999,.T.);
#1864=EDGE_CURVE('',#1543,#1543,#1328,.T.);
#1865=EDGE_CURVE('',#1543,#1544,#1329,.T.);
#1866=EDGE_CURVE('',#1544,#1544,#1330,.T.);
#1867=EDGE_CURVE('',#1544,#1545,#1000,.T.);
#1868=EDGE_CURVE('',#1545,#1545,#1331,.T.);
#1869=EDGE_CURVE('',#1545,#1546,#1332,.T.);
#1870=EDGE_CURVE('',#1546,#1546,#1333,.T.);
#1871=EDGE_CURVE('',#1547,#1547,#1334,.T.);
#1872=EDGE_CURVE('',#1547,#1548,#1001,.T.);
#1873=EDGE_CURVE('',#1549,#1548,#1335,.T.);
#1874=EDGE_CURVE('',#1548,#1549,#1336,.T.);
#1875=EDGE_CURVE('',#1550,#1551,#1337,.T.);
#1876=EDGE_CURVE('',#1551,#1550,#1338,.T.);
#1877=EDGE_CURVE('',#1551,#1552,#1002,.T.);
#1878=EDGE_CURVE('',#1552,#1552,#1339,.T.);
#1879=EDGE_CURVE('',#1553,#1554,#1340,.T.);
#1880=EDGE_CURVE('',#1554,#1549,#1341,.T.);
#1881=EDGE_CURVE('',#1554,#1553,#1342,.T.);
#1882=EDGE_CURVE('',#1555,#1555,#1343,.T.);
#1883=EDGE_CURVE('',#1555,#1556,#1344,.T.);
#1884=EDGE_CURVE('',#1556,#1556,#1345,.T.);
#1885=EDGE_CURVE('',#1556,#1557,#1003,.T.);
#1886=EDGE_CURVE('',#1557,#1557,#1346,.T.);
#1887=EDGE_CURVE('',#1557,#1558,#1347,.T.);
#1888=EDGE_CURVE('',#1558,#1558,#1348,.T.);
#1889=EDGE_CURVE('',#1553,#1559,#1004,.T.);
#1890=EDGE_CURVE('',#1559,#1559,#1349,.T.);
#1891=EDGE_CURVE('',#1560,#1560,#1350,.T.);
#1892=EDGE_CURVE('',#1560,#1561,#1005,.T.);
#1893=EDGE_CURVE('',#1562,#1561,#1351,.T.);
#1894=EDGE_CURVE('',#1561,#1562,#1352,.T.);
#1895=EDGE_CURVE('',#1550,#1562,#1353,.T.);
#1896=EDGE_CURVE('',#1563,#1563,#1354,.T.);
#1897=EDGE_CURVE('',#1563,#1564,#1006,.T.);
#1898=EDGE_CURVE('',#1564,#1564,#1355,.T.);
#1899=EDGE_CURVE('',#1565,#1565,#1356,.T.);
#1900=EDGE_CURVE('',#1565,#1566,#1007,.T.);
#1901=EDGE_CURVE('',#1566,#1566,#1357,.T.);
#1902=EDGE_CURVE('',#1567,#1567,#1358,.T.);
#1903=EDGE_CURVE('',#1567,#1568,#1008,.T.);
#1904=EDGE_CURVE('',#1568,#1568,#1359,.T.);
#1905=EDGE_CURVE('',#1569,#1569,#1360,.T.);
#1906=EDGE_CURVE('',#1569,#1570,#1009,.T.);
#1907=EDGE_CURVE('',#1570,#1570,#1361,.T.);
#1908=EDGE_CURVE('',#1571,#1572,#1010,.T.);
#1909=EDGE_CURVE('',#1572,#1573,#1362,.T.);
#1910=EDGE_CURVE('',#1573,#1574,#1363,.T.);
#1911=EDGE_CURVE('',#1574,#1575,#1364,.T.);
#1912=EDGE_CURVE('',#1575,#1576,#1365,.T.);
#1913=EDGE_CURVE('',#1576,#1577,#1366,.T.);
#1914=EDGE_CURVE('',#1577,#1572,#1367,.T.);
#1915=EDGE_CURVE('',#1578,#1578,#1368,.T.);
#1916=EDGE_CURVE('',#1578,#1579,#1369,.T.);
#1917=EDGE_CURVE('',#1579,#1579,#1370,.T.);
#1918=EDGE_CURVE('',#1580,#1581,#1371,.T.);
#1919=EDGE_CURVE('',#1581,#1580,#1372,.T.);
#1920=EDGE_CURVE('',#1581,#1582,#1373,.T.);
#1921=EDGE_CURVE('',#1582,#1582,#1374,.T.);
#1922=EDGE_CURVE('',#1579,#1583,#1011,.T.);
#1923=EDGE_CURVE('',#1583,#1583,#1375,.T.);
#1924=EDGE_CURVE('',#1580,#1584,#1012,.T.);
#1925=EDGE_CURVE('',#1584,#1584,#1376,.T.);
#1926=EDGE_CURVE('',#1584,#1585,#1013,.T.);
#1927=EDGE_CURVE('',#1585,#1585,#1377,.T.);
#1928=EDGE_CURVE('',#1586,#1587,#1014,.T.);
#1929=EDGE_CURVE('',#1588,#1587,#1015,.T.);
#1930=EDGE_CURVE('',#1588,#1589,#1016,.T.);
#1931=EDGE_CURVE('',#1589,#1590,#1017,.T.);
#1932=EDGE_CURVE('',#1591,#1590,#1018,.T.);
#1933=EDGE_CURVE('',#1586,#1591,#1019,.T.);
#1934=EDGE_CURVE('',#1592,#1586,#1020,.T.);
#1935=EDGE_CURVE('',#1592,#1576,#1021,.T.);
#1936=EDGE_CURVE('',#1576,#1593,#1022,.T.);
#1937=EDGE_CURVE('',#1593,#1587,#1023,.T.);
#1938=EDGE_CURVE('',#1575,#1593,#1024,.T.);
#1939=EDGE_CURVE('',#1594,#1575,#1025,.T.);
#1940=EDGE_CURVE('',#1594,#1588,#1026,.T.);
#1941=EDGE_CURVE('',#1594,#1574,#1027,.T.);
#1942=EDGE_CURVE('',#1574,#1595,#1028,.T.);
#1943=EDGE_CURVE('',#1595,#1589,#1029,.T.);
#1944=EDGE_CURVE('',#1595,#1573,#1030,.T.);
#1945=EDGE_CURVE('',#1573,#1596,#1031,.T.);
#1946=EDGE_CURVE('',#1596,#1590,#1032,.T.);
#1947=EDGE_CURVE('',#1572,#1596,#1033,.T.);
#1948=EDGE_CURVE('',#1597,#1572,#1034,.T.);
#1949=EDGE_CURVE('',#1597,#1591,#1035,.T.);
#1950=EDGE_CURVE('',#1577,#1597,#1036,.T.);
#1951=EDGE_CURVE('',#1592,#1577,#1037,.T.);
#1952=EDGE_CURVE('',#1598,#1598,#1378,.T.);
#1953=EDGE_CURVE('',#1598,#1599,#1038,.T.);
#1954=EDGE_CURVE('',#1599,#1600,#1379,.T.);
#1955=EDGE_CURVE('',#1600,#1599,#1380,.T.);
#1956=EDGE_CURVE('',#1601,#1602,#1381,.T.);
#1957=EDGE_CURVE('',#1602,#1600,#1039,.T.);
#1958=EDGE_CURVE('',#1602,#1601,#1382,.T.);
#1959=EDGE_CURVE('',#1603,#1603,#1383,.T.);
#1960=EDGE_CURVE('',#1603,#1604,#1040,.T.);
#1961=EDGE_CURVE('',#1604,#1604,#1384,.T.);
#1962=EDGE_CURVE('',#1605,#1606,#1385,.T.);
#1963=EDGE_CURVE('',#1606,#1607,#1041,.T.);
#1964=EDGE_CURVE('',#1607,#1608,#217,.T.);
#1965=EDGE_CURVE('',#1608,#1609,#218,.T.);
#1966=EDGE_CURVE('',#1609,#1610,#219,.T.);
#1967=EDGE_CURVE('',#1610,#1611,#220,.T.);
#1968=EDGE_CURVE('',#1611,#1612,#221,.T.);
#1969=EDGE_CURVE('',#1612,#1613,#222,.T.);
#1970=EDGE_CURVE('',#1613,#1614,#223,.T.);
#1971=EDGE_CURVE('',#1614,#1607,#224,.T.);
#1972=EDGE_CURVE('',#1606,#1605,#1386,.T.);
#1973=EDGE_CURVE('',#1605,#1615,#1387,.T.);
#1974=EDGE_CURVE('',#1615,#1615,#1388,.T.);
#1975=EDGE_CURVE('',#1601,#1603,#1042,.T.);
#1976=EDGE_CURVE('',#1616,#1617,#1043,.T.);
#1977=EDGE_CURVE('',#1616,#1618,#225,.T.);
#1978=EDGE_CURVE('',#1618,#1619,#1044,.T.);
#1979=EDGE_CURVE('',#1619,#1620,#205,.T.);
#1980=EDGE_CURVE('',#1620,#1617,#206,.T.);
#1981=EDGE_CURVE('',#1621,#1622,#1045,.T.);
#1982=EDGE_CURVE('',#1621,#1616,#226,.T.);
#1983=EDGE_CURVE('',#1617,#1623,#207,.T.);
#1984=EDGE_CURVE('',#1623,#1622,#208,.T.);
#1985=EDGE_CURVE('',#1624,#1625,#1046,.T.);
#1986=EDGE_CURVE('',#1624,#1621,#227,.T.);
#1987=EDGE_CURVE('',#1626,#1622,#209,.T.);
#1988=EDGE_CURVE('',#1625,#1626,#210,.T.);
#1989=EDGE_CURVE('',#1627,#1628,#1047,.T.);
#1990=EDGE_CURVE('',#1627,#1624,#228,.T.);
#1991=EDGE_CURVE('',#1625,#1629,#211,.T.);
#1992=EDGE_CURVE('',#1629,#1628,#212,.T.);
#1993=EDGE_CURVE('',#1630,#1631,#1048,.T.);
#1994=EDGE_CURVE('',#1630,#1627,#229,.T.);
#1995=EDGE_CURVE('',#1628,#1632,#213,.T.);
#1996=EDGE_CURVE('',#1632,#1631,#214,.T.);
#1997=EDGE_CURVE('',#1618,#1630,#230,.T.);
#1998=EDGE_CURVE('',#1631,#1633,#215,.T.);
#1999=EDGE_CURVE('',#1633,#1619,#216,.T.);
#2000=EDGE_CURVE('',#1633,#1620,#1389,.T.);
#2001=EDGE_CURVE('',#1632,#1633,#1390,.T.);
#2002=EDGE_CURVE('',#1629,#1632,#1391,.T.);
#2003=EDGE_CURVE('',#1626,#1629,#1392,.T.);
#2004=EDGE_CURVE('',#1626,#1623,#1393,.T.);
#2005=EDGE_CURVE('',#1620,#1623,#1394,.T.);
#2006=EDGE_CURVE('',#1610,#1630,#231,.T.);
#2007=EDGE_CURVE('',#1627,#1609,#232,.T.);
#2008=EDGE_CURVE('',#1624,#1608,#233,.T.);
#2009=EDGE_CURVE('',#1612,#1618,#234,.T.);
#2010=EDGE_CURVE('',#1621,#1614,#235,.T.);
#2011=EDGE_CURVE('',#1613,#1616,#236,.T.);
#2012=ORIENTED_EDGE('',*,*,#1634,.F.);
#2013=ORIENTED_EDGE('',*,*,#1635,.T.);
#2014=ORIENTED_EDGE('',*,*,#1636,.T.);
#2015=ORIENTED_EDGE('',*,*,#1637,.F.);
#2016=ORIENTED_EDGE('',*,*,#1638,.F.);
#2017=ORIENTED_EDGE('',*,*,#1639,.T.);
#2018=ORIENTED_EDGE('',*,*,#1640,.T.);
#2019=ORIENTED_EDGE('',*,*,#1641,.F.);
#2020=ORIENTED_EDGE('',*,*,#1642,.T.);
#2021=ORIENTED_EDGE('',*,*,#1643,.T.);
#2022=ORIENTED_EDGE('',*,*,#1644,.F.);
#2023=ORIENTED_EDGE('',*,*,#1643,.F.);
#2024=ORIENTED_EDGE('',*,*,#1645,.T.);
#2025=ORIENTED_EDGE('',*,*,#1646,.T.);
#2026=ORIENTED_EDGE('',*,*,#1647,.F.);
#2027=ORIENTED_EDGE('',*,*,#1646,.F.);
#2028=ORIENTED_EDGE('',*,*,#1648,.T.);
#2029=ORIENTED_EDGE('',*,*,#1649,.T.);
#2030=ORIENTED_EDGE('',*,*,#1650,.F.);
#2031=ORIENTED_EDGE('',*,*,#1649,.F.);
#2032=ORIENTED_EDGE('',*,*,#1651,.T.);
#2033=ORIENTED_EDGE('',*,*,#1652,.T.);
#2034=ORIENTED_EDGE('',*,*,#1653,.F.);
#2035=ORIENTED_EDGE('',*,*,#1652,.F.);
#2036=ORIENTED_EDGE('',*,*,#1654,.T.);
#2037=ORIENTED_EDGE('',*,*,#1655,.T.);
#2038=ORIENTED_EDGE('',*,*,#1656,.F.);
#2039=ORIENTED_EDGE('',*,*,#1655,.F.);
#2040=ORIENTED_EDGE('',*,*,#1657,.F.);
#2041=ORIENTED_EDGE('',*,*,#1658,.T.);
#2042=ORIENTED_EDGE('',*,*,#1659,.T.);
#2043=ORIENTED_EDGE('',*,*,#1658,.F.);
#2044=ORIENTED_EDGE('',*,*,#1660,.F.);
#2045=ORIENTED_EDGE('',*,*,#1661,.T.);
#2046=ORIENTED_EDGE('',*,*,#1662,.T.);
#2047=ORIENTED_EDGE('',*,*,#1661,.F.);
#2048=ORIENTED_EDGE('',*,*,#1663,.F.);
#2049=ORIENTED_EDGE('',*,*,#1664,.T.);
#2050=ORIENTED_EDGE('',*,*,#1665,.T.);
#2051=ORIENTED_EDGE('',*,*,#1664,.F.);
#2052=ORIENTED_EDGE('',*,*,#1666,.F.);
#2053=ORIENTED_EDGE('',*,*,#1667,.T.);
#2054=ORIENTED_EDGE('',*,*,#1668,.T.);
#2055=ORIENTED_EDGE('',*,*,#1667,.F.);
#2056=ORIENTED_EDGE('',*,*,#1669,.F.);
#2057=ORIENTED_EDGE('',*,*,#1670,.T.);
#2058=ORIENTED_EDGE('',*,*,#1671,.T.);
#2059=ORIENTED_EDGE('',*,*,#1670,.F.);
#2060=ORIENTED_EDGE('',*,*,#1672,.F.);
#2061=ORIENTED_EDGE('',*,*,#1673,.T.);
#2062=ORIENTED_EDGE('',*,*,#1674,.T.);
#2063=ORIENTED_EDGE('',*,*,#1675,.F.);
#2064=ORIENTED_EDGE('',*,*,#1676,.F.);
#2065=ORIENTED_EDGE('',*,*,#1677,.T.);
#2066=ORIENTED_EDGE('',*,*,#1678,.T.);
#2067=ORIENTED_EDGE('',*,*,#1679,.F.);
#2068=ORIENTED_EDGE('',*,*,#1642,.F.);
#2069=ORIENTED_EDGE('',*,*,#1645,.F.);
#2070=ORIENTED_EDGE('',*,*,#1648,.F.);
#2071=ORIENTED_EDGE('',*,*,#1651,.F.);
#2072=ORIENTED_EDGE('',*,*,#1654,.F.);
#2073=ORIENTED_EDGE('',*,*,#1680,.T.);
#2074=ORIENTED_EDGE('',*,*,#1681,.T.);
#2075=ORIENTED_EDGE('',*,*,#1682,.F.);
#2076=ORIENTED_EDGE('',*,*,#1683,.F.);
#2077=ORIENTED_EDGE('',*,*,#1657,.T.);
#2078=ORIENTED_EDGE('',*,*,#1660,.T.);
#2079=ORIENTED_EDGE('',*,*,#1663,.T.);
#2080=ORIENTED_EDGE('',*,*,#1666,.T.);
#2081=ORIENTED_EDGE('',*,*,#1669,.T.);
#2082=ORIENTED_EDGE('',*,*,#1684,.F.);
#2083=ORIENTED_EDGE('',*,*,#1685,.F.);
#2084=ORIENTED_EDGE('',*,*,#1686,.T.);
#2085=ORIENTED_EDGE('',*,*,#1682,.T.);
#2086=ORIENTED_EDGE('',*,*,#1687,.F.);
#2087=ORIENTED_EDGE('',*,*,#1688,.T.);
#2088=ORIENTED_EDGE('',*,*,#1689,.T.);
#2089=ORIENTED_EDGE('',*,*,#1675,.T.);
#2090=ORIENTED_EDGE('',*,*,#1690,.F.);
#2091=ORIENTED_EDGE('',*,*,#1691,.T.);
#2092=ORIENTED_EDGE('',*,*,#1692,.T.);
#2093=ORIENTED_EDGE('',*,*,#1679,.T.);
#2094=ORIENTED_EDGE('',*,*,#1693,.F.);
#2095=ORIENTED_EDGE('',*,*,#1694,.F.);
#2096=ORIENTED_EDGE('',*,*,#1695,.T.);
#2097=ORIENTED_EDGE('',*,*,#1685,.T.);
#2098=ORIENTED_EDGE('',*,*,#1644,.T.);
#2099=ORIENTED_EDGE('',*,*,#1647,.T.);
#2100=ORIENTED_EDGE('',*,*,#1650,.T.);
#2101=ORIENTED_EDGE('',*,*,#1653,.T.);
#2102=ORIENTED_EDGE('',*,*,#1656,.T.);
#2103=ORIENTED_EDGE('',*,*,#1659,.F.);
#2104=ORIENTED_EDGE('',*,*,#1662,.F.);
#2105=ORIENTED_EDGE('',*,*,#1665,.F.);
#2106=ORIENTED_EDGE('',*,*,#1668,.F.);
#2107=ORIENTED_EDGE('',*,*,#1671,.F.);
#2108=ORIENTED_EDGE('',*,*,#1696,.F.);
#2109=ORIENTED_EDGE('',*,*,#1677,.F.);
#2110=ORIENTED_EDGE('',*,*,#1697,.F.);
#2111=ORIENTED_EDGE('',*,*,#1698,.T.);
#2112=ORIENTED_EDGE('',*,*,#1699,.T.);
#2113=ORIENTED_EDGE('',*,*,#1673,.F.);
#2114=ORIENTED_EDGE('',*,*,#1700,.F.);
#2115=ORIENTED_EDGE('',*,*,#1701,.T.);
#2116=ORIENTED_EDGE('',*,*,#1702,.T.);
#2117=ORIENTED_EDGE('',*,*,#1680,.F.);
#2118=ORIENTED_EDGE('',*,*,#1703,.T.);
#2119=ORIENTED_EDGE('',*,*,#1694,.T.);
#2120=ORIENTED_EDGE('',*,*,#1683,.T.);
#2121=ORIENTED_EDGE('',*,*,#1686,.F.);
#2122=ORIENTED_EDGE('',*,*,#1695,.F.);
#2123=ORIENTED_EDGE('',*,*,#1703,.F.);
#2124=ORIENTED_EDGE('',*,*,#1678,.F.);
#2125=ORIENTED_EDGE('',*,*,#1696,.T.);
#2126=ORIENTED_EDGE('',*,*,#1693,.T.);
#2127=ORIENTED_EDGE('',*,*,#1684,.T.);
#2128=ORIENTED_EDGE('',*,*,#1676,.T.);
#2129=ORIENTED_EDGE('',*,*,#1692,.F.);
#2130=ORIENTED_EDGE('',*,*,#1704,.F.);
#2131=ORIENTED_EDGE('',*,*,#1697,.T.);
#2132=ORIENTED_EDGE('',*,*,#1705,.T.);
#2133=ORIENTED_EDGE('',*,*,#1706,.T.);
#2134=ORIENTED_EDGE('',*,*,#1707,.T.);
#2135=ORIENTED_EDGE('',*,*,#1634,.T.);
#2136=ORIENTED_EDGE('',*,*,#1674,.F.);
#2137=ORIENTED_EDGE('',*,*,#1699,.F.);
#2138=ORIENTED_EDGE('',*,*,#1708,.T.);
#2139=ORIENTED_EDGE('',*,*,#1690,.T.);
#2140=ORIENTED_EDGE('',*,*,#1709,.F.);
#2141=ORIENTED_EDGE('',*,*,#1710,.F.);
#2142=ORIENTED_EDGE('',*,*,#1636,.F.);
#2143=ORIENTED_EDGE('',*,*,#1711,.F.);
#2144=ORIENTED_EDGE('',*,*,#1704,.T.);
#2145=ORIENTED_EDGE('',*,*,#1691,.F.);
#2146=ORIENTED_EDGE('',*,*,#1708,.F.);
#2147=ORIENTED_EDGE('',*,*,#1698,.F.);
#2148=ORIENTED_EDGE('',*,*,#1672,.T.);
#2149=ORIENTED_EDGE('',*,*,#1689,.F.);
#2150=ORIENTED_EDGE('',*,*,#1712,.F.);
#2151=ORIENTED_EDGE('',*,*,#1700,.T.);
#2152=ORIENTED_EDGE('',*,*,#1713,.T.);
#2153=ORIENTED_EDGE('',*,*,#1714,.T.);
#2154=ORIENTED_EDGE('',*,*,#1715,.T.);
#2155=ORIENTED_EDGE('',*,*,#1638,.T.);
#2156=ORIENTED_EDGE('',*,*,#1681,.F.);
#2157=ORIENTED_EDGE('',*,*,#1702,.F.);
#2158=ORIENTED_EDGE('',*,*,#1716,.T.);
#2159=ORIENTED_EDGE('',*,*,#1687,.T.);
#2160=ORIENTED_EDGE('',*,*,#1717,.F.);
#2161=ORIENTED_EDGE('',*,*,#1718,.F.);
#2162=ORIENTED_EDGE('',*,*,#1640,.F.);
#2163=ORIENTED_EDGE('',*,*,#1719,.F.);
#2164=ORIENTED_EDGE('',*,*,#1712,.T.);
#2165=ORIENTED_EDGE('',*,*,#1688,.F.);
#2166=ORIENTED_EDGE('',*,*,#1716,.F.);
#2167=ORIENTED_EDGE('',*,*,#1701,.F.);
#2168=ORIENTED_EDGE('',*,*,#1720,.T.);
#2169=ORIENTED_EDGE('',*,*,#1719,.T.);
#2170=ORIENTED_EDGE('',*,*,#1639,.F.);
#2171=ORIENTED_EDGE('',*,*,#1715,.F.);
#2172=ORIENTED_EDGE('',*,*,#1641,.T.);
#2173=ORIENTED_EDGE('',*,*,#1718,.T.);
#2174=ORIENTED_EDGE('',*,*,#1721,.F.);
#2175=ORIENTED_EDGE('',*,*,#1713,.F.);
#2176=ORIENTED_EDGE('',*,*,#1721,.T.);
#2177=ORIENTED_EDGE('',*,*,#1717,.T.);
#2178=ORIENTED_EDGE('',*,*,#1720,.F.);
#2179=ORIENTED_EDGE('',*,*,#1714,.F.);
#2180=ORIENTED_EDGE('',*,*,#1722,.T.);
#2181=ORIENTED_EDGE('',*,*,#1709,.T.);
#2182=ORIENTED_EDGE('',*,*,#1723,.F.);
#2183=ORIENTED_EDGE('',*,*,#1706,.F.);
#2184=ORIENTED_EDGE('',*,*,#1637,.T.);
#2185=ORIENTED_EDGE('',*,*,#1710,.T.);
#2186=ORIENTED_EDGE('',*,*,#1722,.F.);
#2187=ORIENTED_EDGE('',*,*,#1705,.F.);
#2188=ORIENTED_EDGE('',*,*,#1723,.T.);
#2189=ORIENTED_EDGE('',*,*,#1711,.T.);
#2190=ORIENTED_EDGE('',*,*,#1635,.F.);
#2191=ORIENTED_EDGE('',*,*,#1707,.F.);
#2192=ORIENTED_EDGE('',*,*,#1724,.F.);
#2193=ORIENTED_EDGE('',*,*,#1725,.T.);
#2194=ORIENTED_EDGE('',*,*,#1726,.T.);
#2195=ORIENTED_EDGE('',*,*,#1725,.F.);
#2196=ORIENTED_EDGE('',*,*,#1727,.F.);
#2197=ORIENTED_EDGE('',*,*,#1728,.T.);
#2198=ORIENTED_EDGE('',*,*,#1729,.T.);
#2199=ORIENTED_EDGE('',*,*,#1728,.F.);
#2200=ORIENTED_EDGE('',*,*,#1730,.F.);
#2201=ORIENTED_EDGE('',*,*,#1731,.T.);
#2202=ORIENTED_EDGE('',*,*,#1732,.T.);
#2203=ORIENTED_EDGE('',*,*,#1731,.F.);
#2204=ORIENTED_EDGE('',*,*,#1733,.F.);
#2205=ORIENTED_EDGE('',*,*,#1734,.T.);
#2206=ORIENTED_EDGE('',*,*,#1735,.T.);
#2207=ORIENTED_EDGE('',*,*,#1734,.F.);
#2208=ORIENTED_EDGE('',*,*,#1736,.F.);
#2209=ORIENTED_EDGE('',*,*,#1737,.T.);
#2210=ORIENTED_EDGE('',*,*,#1738,.T.);
#2211=ORIENTED_EDGE('',*,*,#1737,.F.);
#2212=ORIENTED_EDGE('',*,*,#1739,.T.);
#2213=ORIENTED_EDGE('',*,*,#1740,.T.);
#2214=ORIENTED_EDGE('',*,*,#1741,.F.);
#2215=ORIENTED_EDGE('',*,*,#1742,.F.);
#2216=ORIENTED_EDGE('',*,*,#1741,.T.);
#2217=ORIENTED_EDGE('',*,*,#1743,.T.);
#2218=ORIENTED_EDGE('',*,*,#1744,.F.);
#2219=ORIENTED_EDGE('',*,*,#1745,.F.);
#2220=ORIENTED_EDGE('',*,*,#1744,.T.);
#2221=ORIENTED_EDGE('',*,*,#1746,.T.);
#2222=ORIENTED_EDGE('',*,*,#1747,.F.);
#2223=ORIENTED_EDGE('',*,*,#1748,.F.);
#2224=ORIENTED_EDGE('',*,*,#1747,.T.);
#2225=ORIENTED_EDGE('',*,*,#1749,.T.);
#2226=ORIENTED_EDGE('',*,*,#1739,.F.);
#2227=ORIENTED_EDGE('',*,*,#1750,.F.);
#2228=ORIENTED_EDGE('',*,*,#1751,.T.);
#2229=ORIENTED_EDGE('',*,*,#1752,.T.);
#2230=ORIENTED_EDGE('',*,*,#1753,.F.);
#2231=ORIENTED_EDGE('',*,*,#1754,.F.);
#2232=ORIENTED_EDGE('',*,*,#1753,.T.);
#2233=ORIENTED_EDGE('',*,*,#1755,.T.);
#2234=ORIENTED_EDGE('',*,*,#1756,.F.);
#2235=ORIENTED_EDGE('',*,*,#1757,.F.);
#2236=ORIENTED_EDGE('',*,*,#1756,.T.);
#2237=ORIENTED_EDGE('',*,*,#1758,.T.);
#2238=ORIENTED_EDGE('',*,*,#1759,.F.);
#2239=ORIENTED_EDGE('',*,*,#1760,.F.);
#2240=ORIENTED_EDGE('',*,*,#1759,.T.);
#2241=ORIENTED_EDGE('',*,*,#1761,.T.);
#2242=ORIENTED_EDGE('',*,*,#1751,.F.);
#2243=ORIENTED_EDGE('',*,*,#1762,.F.);
#2244=ORIENTED_EDGE('',*,*,#1763,.T.);
#2245=ORIENTED_EDGE('',*,*,#1764,.T.);
#2246=ORIENTED_EDGE('',*,*,#1765,.F.);
#2247=ORIENTED_EDGE('',*,*,#1766,.F.);
#2248=ORIENTED_EDGE('',*,*,#1765,.T.);
#2249=ORIENTED_EDGE('',*,*,#1767,.T.);
#2250=ORIENTED_EDGE('',*,*,#1768,.F.);
#2251=ORIENTED_EDGE('',*,*,#1769,.F.);
#2252=ORIENTED_EDGE('',*,*,#1768,.T.);
#2253=ORIENTED_EDGE('',*,*,#1770,.T.);
#2254=ORIENTED_EDGE('',*,*,#1771,.F.);
#2255=ORIENTED_EDGE('',*,*,#1772,.F.);
#2256=ORIENTED_EDGE('',*,*,#1771,.T.);
#2257=ORIENTED_EDGE('',*,*,#1773,.T.);
#2258=ORIENTED_EDGE('',*,*,#1763,.F.);
#2259=ORIENTED_EDGE('',*,*,#1774,.F.);
#2260=ORIENTED_EDGE('',*,*,#1775,.T.);
#2261=ORIENTED_EDGE('',*,*,#1776,.T.);
#2262=ORIENTED_EDGE('',*,*,#1777,.F.);
#2263=ORIENTED_EDGE('',*,*,#1778,.F.);
#2264=ORIENTED_EDGE('',*,*,#1777,.T.);
#2265=ORIENTED_EDGE('',*,*,#1779,.T.);
#2266=ORIENTED_EDGE('',*,*,#1780,.F.);
#2267=ORIENTED_EDGE('',*,*,#1781,.F.);
#2268=ORIENTED_EDGE('',*,*,#1780,.T.);
#2269=ORIENTED_EDGE('',*,*,#1782,.T.);
#2270=ORIENTED_EDGE('',*,*,#1783,.F.);
#2271=ORIENTED_EDGE('',*,*,#1784,.F.);
#2272=ORIENTED_EDGE('',*,*,#1783,.T.);
#2273=ORIENTED_EDGE('',*,*,#1785,.T.);
#2274=ORIENTED_EDGE('',*,*,#1775,.F.);
#2275=ORIENTED_EDGE('',*,*,#1786,.F.);
#2276=ORIENTED_EDGE('',*,*,#1787,.T.);
#2277=ORIENTED_EDGE('',*,*,#1788,.T.);
#2278=ORIENTED_EDGE('',*,*,#1789,.T.);
#2279=ORIENTED_EDGE('',*,*,#1790,.F.);
#2280=ORIENTED_EDGE('',*,*,#1791,.F.);
#2281=ORIENTED_EDGE('',*,*,#1792,.T.);
#2282=ORIENTED_EDGE('',*,*,#1793,.T.);
#2283=ORIENTED_EDGE('',*,*,#1794,.F.);
#2284=ORIENTED_EDGE('',*,*,#1795,.F.);
#2285=ORIENTED_EDGE('',*,*,#1796,.F.);
#2286=ORIENTED_EDGE('',*,*,#1797,.F.);
#2287=ORIENTED_EDGE('',*,*,#1798,.T.);
#2288=ORIENTED_EDGE('',*,*,#1799,.T.);
#2289=ORIENTED_EDGE('',*,*,#1792,.F.);
#2290=ORIENTED_EDGE('',*,*,#1800,.F.);
#2291=ORIENTED_EDGE('',*,*,#1794,.T.);
#2292=ORIENTED_EDGE('',*,*,#1791,.T.);
#2293=ORIENTED_EDGE('',*,*,#1801,.F.);
#2294=ORIENTED_EDGE('',*,*,#1795,.T.);
#2295=ORIENTED_EDGE('',*,*,#1800,.T.);
#2296=ORIENTED_EDGE('',*,*,#1785,.F.);
#2297=ORIENTED_EDGE('',*,*,#1782,.F.);
#2298=ORIENTED_EDGE('',*,*,#1779,.F.);
#2299=ORIENTED_EDGE('',*,*,#1776,.F.);
#2300=ORIENTED_EDGE('',*,*,#1773,.F.);
#2301=ORIENTED_EDGE('',*,*,#1770,.F.);
#2302=ORIENTED_EDGE('',*,*,#1767,.F.);
#2303=ORIENTED_EDGE('',*,*,#1764,.F.);
#2304=ORIENTED_EDGE('',*,*,#1761,.F.);
#2305=ORIENTED_EDGE('',*,*,#1758,.F.);
#2306=ORIENTED_EDGE('',*,*,#1755,.F.);
#2307=ORIENTED_EDGE('',*,*,#1752,.F.);
#2308=ORIENTED_EDGE('',*,*,#1749,.F.);
#2309=ORIENTED_EDGE('',*,*,#1746,.F.);
#2310=ORIENTED_EDGE('',*,*,#1743,.F.);
#2311=ORIENTED_EDGE('',*,*,#1740,.F.);
#2312=ORIENTED_EDGE('',*,*,#1802,.F.);
#2313=ORIENTED_EDGE('',*,*,#1803,.F.);
#2314=ORIENTED_EDGE('',*,*,#1804,.F.);
#2315=ORIENTED_EDGE('',*,*,#1805,.F.);
#2316=ORIENTED_EDGE('',*,*,#1806,.F.);
#2317=ORIENTED_EDGE('',*,*,#1807,.F.);
#2318=ORIENTED_EDGE('',*,*,#1808,.F.);
#2319=ORIENTED_EDGE('',*,*,#1809,.F.);
#2320=ORIENTED_EDGE('',*,*,#1787,.F.);
#2321=ORIENTED_EDGE('',*,*,#1799,.F.);
#2322=ORIENTED_EDGE('',*,*,#1793,.F.);
#2323=ORIENTED_EDGE('',*,*,#1810,.F.);
#2324=ORIENTED_EDGE('',*,*,#1786,.T.);
#2325=ORIENTED_EDGE('',*,*,#1778,.T.);
#2326=ORIENTED_EDGE('',*,*,#1781,.T.);
#2327=ORIENTED_EDGE('',*,*,#1784,.T.);
#2328=ORIENTED_EDGE('',*,*,#1774,.T.);
#2329=ORIENTED_EDGE('',*,*,#1766,.T.);
#2330=ORIENTED_EDGE('',*,*,#1769,.T.);
#2331=ORIENTED_EDGE('',*,*,#1772,.T.);
#2332=ORIENTED_EDGE('',*,*,#1762,.T.);
#2333=ORIENTED_EDGE('',*,*,#1754,.T.);
#2334=ORIENTED_EDGE('',*,*,#1757,.T.);
#2335=ORIENTED_EDGE('',*,*,#1760,.T.);
#2336=ORIENTED_EDGE('',*,*,#1750,.T.);
#2337=ORIENTED_EDGE('',*,*,#1742,.T.);
#2338=ORIENTED_EDGE('',*,*,#1745,.T.);
#2339=ORIENTED_EDGE('',*,*,#1748,.T.);
#2340=ORIENTED_EDGE('',*,*,#1811,.T.);
#2341=ORIENTED_EDGE('',*,*,#1812,.T.);
#2342=ORIENTED_EDGE('',*,*,#1813,.T.);
#2343=ORIENTED_EDGE('',*,*,#1814,.T.);
#2344=ORIENTED_EDGE('',*,*,#1815,.T.);
#2345=ORIENTED_EDGE('',*,*,#1816,.T.);
#2346=ORIENTED_EDGE('',*,*,#1817,.T.);
#2347=ORIENTED_EDGE('',*,*,#1818,.T.);
#2348=ORIENTED_EDGE('',*,*,#1819,.F.);
#2349=ORIENTED_EDGE('',*,*,#1789,.F.);
#2350=ORIENTED_EDGE('',*,*,#1820,.T.);
#2351=ORIENTED_EDGE('',*,*,#1797,.T.);
#2352=ORIENTED_EDGE('',*,*,#1810,.T.);
#2353=ORIENTED_EDGE('',*,*,#1798,.F.);
#2354=ORIENTED_EDGE('',*,*,#1820,.F.);
#2355=ORIENTED_EDGE('',*,*,#1788,.F.);
#2356=ORIENTED_EDGE('',*,*,#1724,.T.);
#2357=ORIENTED_EDGE('',*,*,#1727,.T.);
#2358=ORIENTED_EDGE('',*,*,#1730,.T.);
#2359=ORIENTED_EDGE('',*,*,#1733,.T.);
#2360=ORIENTED_EDGE('',*,*,#1736,.T.);
#2361=ORIENTED_EDGE('',*,*,#1796,.T.);
#2362=ORIENTED_EDGE('',*,*,#1801,.T.);
#2363=ORIENTED_EDGE('',*,*,#1790,.T.);
#2364=ORIENTED_EDGE('',*,*,#1819,.T.);
#2365=ORIENTED_EDGE('',*,*,#1726,.F.);
#2366=ORIENTED_EDGE('',*,*,#1729,.F.);
#2367=ORIENTED_EDGE('',*,*,#1732,.F.);
#2368=ORIENTED_EDGE('',*,*,#1735,.F.);
#2369=ORIENTED_EDGE('',*,*,#1738,.F.);
#2370=ORIENTED_EDGE('',*,*,#1821,.T.);
#2371=ORIENTED_EDGE('',*,*,#1807,.T.);
#2372=ORIENTED_EDGE('',*,*,#1822,.F.);
#2373=ORIENTED_EDGE('',*,*,#1815,.F.);
#2374=ORIENTED_EDGE('',*,*,#1823,.T.);
#2375=ORIENTED_EDGE('',*,*,#1808,.T.);
#2376=ORIENTED_EDGE('',*,*,#1821,.F.);
#2377=ORIENTED_EDGE('',*,*,#1818,.F.);
#2378=ORIENTED_EDGE('',*,*,#1824,.T.);
#2379=ORIENTED_EDGE('',*,*,#1809,.T.);
#2380=ORIENTED_EDGE('',*,*,#1823,.F.);
#2381=ORIENTED_EDGE('',*,*,#1817,.F.);
#2382=ORIENTED_EDGE('',*,*,#1822,.T.);
#2383=ORIENTED_EDGE('',*,*,#1806,.T.);
#2384=ORIENTED_EDGE('',*,*,#1824,.F.);
#2385=ORIENTED_EDGE('',*,*,#1816,.F.);
#2386=ORIENTED_EDGE('',*,*,#1825,.T.);
#2387=ORIENTED_EDGE('',*,*,#1803,.T.);
#2388=ORIENTED_EDGE('',*,*,#1826,.F.);
#2389=ORIENTED_EDGE('',*,*,#1811,.F.);
#2390=ORIENTED_EDGE('',*,*,#1827,.T.);
#2391=ORIENTED_EDGE('',*,*,#1804,.T.);
#2392=ORIENTED_EDGE('',*,*,#1825,.F.);
#2393=ORIENTED_EDGE('',*,*,#1814,.F.);
#2394=ORIENTED_EDGE('',*,*,#1828,.T.);
#2395=ORIENTED_EDGE('',*,*,#1805,.T.);
#2396=ORIENTED_EDGE('',*,*,#1827,.F.);
#2397=ORIENTED_EDGE('',*,*,#1813,.F.);
#2398=ORIENTED_EDGE('',*,*,#1826,.T.);
#2399=ORIENTED_EDGE('',*,*,#1802,.T.);
#2400=ORIENTED_EDGE('',*,*,#1828,.F.);
#2401=ORIENTED_EDGE('',*,*,#1812,.F.);
#2402=ORIENTED_EDGE('',*,*,#1829,.T.);
#2403=ORIENTED_EDGE('',*,*,#1830,.T.);
#2404=ORIENTED_EDGE('',*,*,#1831,.T.);
#2405=ORIENTED_EDGE('',*,*,#1832,.T.);
#2406=ORIENTED_EDGE('',*,*,#1833,.F.);
#2407=ORIENTED_EDGE('',*,*,#1834,.F.);
#2408=ORIENTED_EDGE('',*,*,#1835,.F.);
#2409=ORIENTED_EDGE('',*,*,#1836,.F.);
#2410=ORIENTED_EDGE('',*,*,#1837,.F.);
#2411=ORIENTED_EDGE('',*,*,#1832,.F.);
#2412=ORIENTED_EDGE('',*,*,#1838,.T.);
#2413=ORIENTED_EDGE('',*,*,#1839,.T.);
#2414=ORIENTED_EDGE('',*,*,#1833,.T.);
#2415=ORIENTED_EDGE('',*,*,#1837,.T.);
#2416=ORIENTED_EDGE('',*,*,#1840,.T.);
#2417=ORIENTED_EDGE('',*,*,#1836,.T.);
#2418=ORIENTED_EDGE('',*,*,#1841,.T.);
#2419=ORIENTED_EDGE('',*,*,#1835,.T.);
#2420=ORIENTED_EDGE('',*,*,#1842,.T.);
#2421=ORIENTED_EDGE('',*,*,#1834,.T.);
#2422=ORIENTED_EDGE('',*,*,#1843,.T.);
#2423=ORIENTED_EDGE('',*,*,#1844,.F.);
#2424=ORIENTED_EDGE('',*,*,#1838,.F.);
#2425=ORIENTED_EDGE('',*,*,#1831,.F.);
#2426=ORIENTED_EDGE('',*,*,#1845,.F.);
#2427=ORIENTED_EDGE('',*,*,#1839,.F.);
#2428=ORIENTED_EDGE('',*,*,#1846,.F.);
#2429=ORIENTED_EDGE('',*,*,#1829,.F.);
#2430=ORIENTED_EDGE('',*,*,#1847,.F.);
#2431=ORIENTED_EDGE('',*,*,#1830,.F.);
#2432=ORIENTED_EDGE('',*,*,#1848,.F.);
#2433=ORIENTED_EDGE('',*,*,#1849,.F.);
#2434=ORIENTED_EDGE('',*,*,#1850,.F.);
#2435=ORIENTED_EDGE('',*,*,#1851,.F.);
#2436=ORIENTED_EDGE('',*,*,#1852,.F.);
#2437=ORIENTED_EDGE('',*,*,#1847,.T.);
#2438=ORIENTED_EDGE('',*,*,#1853,.T.);
#2439=ORIENTED_EDGE('',*,*,#1849,.T.);
#2440=ORIENTED_EDGE('',*,*,#1853,.F.);
#2441=ORIENTED_EDGE('',*,*,#1846,.T.);
#2442=ORIENTED_EDGE('',*,*,#1854,.T.);
#2443=ORIENTED_EDGE('',*,*,#1850,.T.);
#2444=ORIENTED_EDGE('',*,*,#1854,.F.);
#2445=ORIENTED_EDGE('',*,*,#1845,.T.);
#2446=ORIENTED_EDGE('',*,*,#1855,.T.);
#2447=ORIENTED_EDGE('',*,*,#1851,.T.);
#2448=ORIENTED_EDGE('',*,*,#1855,.F.);
#2449=ORIENTED_EDGE('',*,*,#1844,.T.);
#2450=ORIENTED_EDGE('',*,*,#1852,.T.);
#2451=ORIENTED_EDGE('',*,*,#1848,.T.);
#2452=ORIENTED_EDGE('',*,*,#1840,.F.);
#2453=ORIENTED_EDGE('',*,*,#1856,.F.);
#2454=ORIENTED_EDGE('',*,*,#1857,.F.);
#2455=ORIENTED_EDGE('',*,*,#1858,.T.);
#2456=ORIENTED_EDGE('',*,*,#1841,.F.);
#2457=ORIENTED_EDGE('',*,*,#1859,.F.);
#2458=ORIENTED_EDGE('',*,*,#1860,.F.);
#2459=ORIENTED_EDGE('',*,*,#1856,.T.);
#2460=ORIENTED_EDGE('',*,*,#1842,.F.);
#2461=ORIENTED_EDGE('',*,*,#1861,.F.);
#2462=ORIENTED_EDGE('',*,*,#1862,.F.);
#2463=ORIENTED_EDGE('',*,*,#1859,.T.);
#2464=ORIENTED_EDGE('',*,*,#1843,.F.);
#2465=ORIENTED_EDGE('',*,*,#1858,.F.);
#2466=ORIENTED_EDGE('',*,*,#1863,.F.);
#2467=ORIENTED_EDGE('',*,*,#1861,.T.);
#2468=ORIENTED_EDGE('',*,*,#1857,.T.);
#2469=ORIENTED_EDGE('',*,*,#1860,.T.);
#2470=ORIENTED_EDGE('',*,*,#1862,.T.);
#2471=ORIENTED_EDGE('',*,*,#1863,.T.);
#2472=ORIENTED_EDGE('',*,*,#1864,.F.);
#2473=ORIENTED_EDGE('',*,*,#1865,.T.);
#2474=ORIENTED_EDGE('',*,*,#1866,.T.);
#2475=ORIENTED_EDGE('',*,*,#1865,.F.);
#2476=ORIENTED_EDGE('',*,*,#1866,.F.);
#2477=ORIENTED_EDGE('',*,*,#1867,.T.);
#2478=ORIENTED_EDGE('',*,*,#1868,.T.);
#2479=ORIENTED_EDGE('',*,*,#1867,.F.);
#2480=ORIENTED_EDGE('',*,*,#1868,.F.);
#2481=ORIENTED_EDGE('',*,*,#1869,.T.);
#2482=ORIENTED_EDGE('',*,*,#1870,.T.);
#2483=ORIENTED_EDGE('',*,*,#1869,.F.);
#2484=ORIENTED_EDGE('',*,*,#1871,.F.);
#2485=ORIENTED_EDGE('',*,*,#1872,.T.);
#2486=ORIENTED_EDGE('',*,*,#1873,.F.);
#2487=ORIENTED_EDGE('',*,*,#1874,.F.);
#2488=ORIENTED_EDGE('',*,*,#1872,.F.);
#2489=ORIENTED_EDGE('',*,*,#1875,.F.);
#2490=ORIENTED_EDGE('',*,*,#1876,.F.);
#2491=ORIENTED_EDGE('',*,*,#1877,.T.);
#2492=ORIENTED_EDGE('',*,*,#1878,.T.);
#2493=ORIENTED_EDGE('',*,*,#1877,.F.);
#2494=ORIENTED_EDGE('',*,*,#1879,.T.);
#2495=ORIENTED_EDGE('',*,*,#1880,.T.);
#2496=ORIENTED_EDGE('',*,*,#1873,.T.);
#2497=ORIENTED_EDGE('',*,*,#1874,.T.);
#2498=ORIENTED_EDGE('',*,*,#1880,.F.);
#2499=ORIENTED_EDGE('',*,*,#1881,.T.);
#2500=ORIENTED_EDGE('',*,*,#1882,.F.);
#2501=ORIENTED_EDGE('',*,*,#1883,.T.);
#2502=ORIENTED_EDGE('',*,*,#1884,.T.);
#2503=ORIENTED_EDGE('',*,*,#1883,.F.);
#2504=ORIENTED_EDGE('',*,*,#1884,.F.);
#2505=ORIENTED_EDGE('',*,*,#1885,.T.);
#2506=ORIENTED_EDGE('',*,*,#1886,.T.);
#2507=ORIENTED_EDGE('',*,*,#1885,.F.);
#2508=ORIENTED_EDGE('',*,*,#1886,.F.);
#2509=ORIENTED_EDGE('',*,*,#1887,.T.);
#2510=ORIENTED_EDGE('',*,*,#1888,.T.);
#2511=ORIENTED_EDGE('',*,*,#1887,.F.);
#2512=ORIENTED_EDGE('',*,*,#1879,.F.);
#2513=ORIENTED_EDGE('',*,*,#1889,.T.);
#2514=ORIENTED_EDGE('',*,*,#1890,.T.);
#2515=ORIENTED_EDGE('',*,*,#1889,.F.);
#2516=ORIENTED_EDGE('',*,*,#1881,.F.);
#2517=ORIENTED_EDGE('',*,*,#1891,.F.);
#2518=ORIENTED_EDGE('',*,*,#1892,.T.);
#2519=ORIENTED_EDGE('',*,*,#1893,.F.);
#2520=ORIENTED_EDGE('',*,*,#1894,.F.);
#2521=ORIENTED_EDGE('',*,*,#1892,.F.);
#2522=ORIENTED_EDGE('',*,*,#1875,.T.);
#2523=ORIENTED_EDGE('',*,*,#1876,.T.);
#2524=ORIENTED_EDGE('',*,*,#1895,.T.);
#2525=ORIENTED_EDGE('',*,*,#1893,.T.);
#2526=ORIENTED_EDGE('',*,*,#1894,.T.);
#2527=ORIENTED_EDGE('',*,*,#1895,.F.);
#2528=ORIENTED_EDGE('',*,*,#1891,.T.);
#2529=ORIENTED_EDGE('',*,*,#1888,.F.);
#2530=ORIENTED_EDGE('',*,*,#1890,.F.);
#2531=ORIENTED_EDGE('',*,*,#1882,.T.);
#2532=ORIENTED_EDGE('',*,*,#1864,.T.);
#2533=ORIENTED_EDGE('',*,*,#1878,.F.);
#2534=ORIENTED_EDGE('',*,*,#1870,.F.);
#2535=ORIENTED_EDGE('',*,*,#1871,.T.);
#2536=ORIENTED_EDGE('',*,*,#1896,.T.);
#2537=ORIENTED_EDGE('',*,*,#1897,.T.);
#2538=ORIENTED_EDGE('',*,*,#1898,.F.);
#2539=ORIENTED_EDGE('',*,*,#1897,.F.);
#2540=ORIENTED_EDGE('',*,*,#1899,.F.);
#2541=ORIENTED_EDGE('',*,*,#1900,.T.);
#2542=ORIENTED_EDGE('',*,*,#1901,.T.);
#2543=ORIENTED_EDGE('',*,*,#1900,.F.);
#2544=ORIENTED_EDGE('',*,*,#1902,.T.);
#2545=ORIENTED_EDGE('',*,*,#1903,.T.);
#2546=ORIENTED_EDGE('',*,*,#1904,.F.);
#2547=ORIENTED_EDGE('',*,*,#1903,.F.);
#2548=ORIENTED_EDGE('',*,*,#1905,.T.);
#2549=ORIENTED_EDGE('',*,*,#1906,.T.);
#2550=ORIENTED_EDGE('',*,*,#1907,.T.);
#2551=ORIENTED_EDGE('',*,*,#1906,.F.);
#2552=ORIENTED_EDGE('',*,*,#1904,.T.);
#2553=ORIENTED_EDGE('',*,*,#1901,.F.);
#2554=ORIENTED_EDGE('',*,*,#1902,.F.);
#2555=ORIENTED_EDGE('',*,*,#1898,.T.);
#2556=ORIENTED_EDGE('',*,*,#1899,.T.);
#2557=ORIENTED_EDGE('',*,*,#1905,.F.);
#2558=ORIENTED_EDGE('',*,*,#1896,.F.);
#2559=ORIENTED_EDGE('',*,*,#1907,.F.);
#2560=ORIENTED_EDGE('',*,*,#1908,.T.);
#2561=ORIENTED_EDGE('',*,*,#1909,.T.);
#2562=ORIENTED_EDGE('',*,*,#1910,.T.);
#2563=ORIENTED_EDGE('',*,*,#1911,.T.);
#2564=ORIENTED_EDGE('',*,*,#1912,.T.);
#2565=ORIENTED_EDGE('',*,*,#1913,.T.);
#2566=ORIENTED_EDGE('',*,*,#1914,.T.);
#2567=ORIENTED_EDGE('',*,*,#1908,.F.);
#2568=ORIENTED_EDGE('',*,*,#1915,.F.);
#2569=ORIENTED_EDGE('',*,*,#1916,.T.);
#2570=ORIENTED_EDGE('',*,*,#1917,.F.);
#2571=ORIENTED_EDGE('',*,*,#1916,.F.);
#2572=ORIENTED_EDGE('',*,*,#1918,.F.);
#2573=ORIENTED_EDGE('',*,*,#1919,.F.);
#2574=ORIENTED_EDGE('',*,*,#1920,.T.);
#2575=ORIENTED_EDGE('',*,*,#1921,.F.);
#2576=ORIENTED_EDGE('',*,*,#1920,.F.);
#2577=ORIENTED_EDGE('',*,*,#1917,.T.);
#2578=ORIENTED_EDGE('',*,*,#1922,.T.);
#2579=ORIENTED_EDGE('',*,*,#1923,.T.);
#2580=ORIENTED_EDGE('',*,*,#1922,.F.);
#2581=ORIENTED_EDGE('',*,*,#1918,.T.);
#2582=ORIENTED_EDGE('',*,*,#1919,.T.);
#2583=ORIENTED_EDGE('',*,*,#1924,.T.);
#2584=ORIENTED_EDGE('',*,*,#1925,.T.);
#2585=ORIENTED_EDGE('',*,*,#1924,.F.);
#2586=ORIENTED_EDGE('',*,*,#1925,.F.);
#2587=ORIENTED_EDGE('',*,*,#1926,.T.);
#2588=ORIENTED_EDGE('',*,*,#1927,.T.);
#2589=ORIENTED_EDGE('',*,*,#1926,.F.);
#2590=ORIENTED_EDGE('',*,*,#1915,.T.);
#2591=ORIENTED_EDGE('',*,*,#1928,.T.);
#2592=ORIENTED_EDGE('',*,*,#1929,.F.);
#2593=ORIENTED_EDGE('',*,*,#1930,.T.);
#2594=ORIENTED_EDGE('',*,*,#1931,.T.);
#2595=ORIENTED_EDGE('',*,*,#1932,.F.);
#2596=ORIENTED_EDGE('',*,*,#1933,.F.);
#2597=ORIENTED_EDGE('',*,*,#1927,.F.);
#2598=ORIENTED_EDGE('',*,*,#1923,.F.);
#2599=ORIENTED_EDGE('',*,*,#1921,.T.);
#2600=ORIENTED_EDGE('',*,*,#1928,.F.);
#2601=ORIENTED_EDGE('',*,*,#1934,.F.);
#2602=ORIENTED_EDGE('',*,*,#1935,.T.);
#2603=ORIENTED_EDGE('',*,*,#1936,.T.);
#2604=ORIENTED_EDGE('',*,*,#1937,.T.);
#2605=ORIENTED_EDGE('',*,*,#1929,.T.);
#2606=ORIENTED_EDGE('',*,*,#1937,.F.);
#2607=ORIENTED_EDGE('',*,*,#1938,.F.);
#2608=ORIENTED_EDGE('',*,*,#1939,.F.);
#2609=ORIENTED_EDGE('',*,*,#1940,.T.);
#2610=ORIENTED_EDGE('',*,*,#1930,.F.);
#2611=ORIENTED_EDGE('',*,*,#1940,.F.);
#2612=ORIENTED_EDGE('',*,*,#1941,.T.);
#2613=ORIENTED_EDGE('',*,*,#1942,.T.);
#2614=ORIENTED_EDGE('',*,*,#1943,.T.);
#2615=ORIENTED_EDGE('',*,*,#1931,.F.);
#2616=ORIENTED_EDGE('',*,*,#1943,.F.);
#2617=ORIENTED_EDGE('',*,*,#1944,.T.);
#2618=ORIENTED_EDGE('',*,*,#1945,.T.);
#2619=ORIENTED_EDGE('',*,*,#1946,.T.);
#2620=ORIENTED_EDGE('',*,*,#1932,.T.);
#2621=ORIENTED_EDGE('',*,*,#1946,.F.);
#2622=ORIENTED_EDGE('',*,*,#1947,.F.);
#2623=ORIENTED_EDGE('',*,*,#1948,.F.);
#2624=ORIENTED_EDGE('',*,*,#1949,.T.);
#2625=ORIENTED_EDGE('',*,*,#1933,.T.);
#2626=ORIENTED_EDGE('',*,*,#1949,.F.);
#2627=ORIENTED_EDGE('',*,*,#1950,.F.);
#2628=ORIENTED_EDGE('',*,*,#1951,.F.);
#2629=ORIENTED_EDGE('',*,*,#1934,.T.);
#2630=ORIENTED_EDGE('',*,*,#1947,.T.);
#2631=ORIENTED_EDGE('',*,*,#1945,.F.);
#2632=ORIENTED_EDGE('',*,*,#1909,.F.);
#2633=ORIENTED_EDGE('',*,*,#1944,.F.);
#2634=ORIENTED_EDGE('',*,*,#1942,.F.);
#2635=ORIENTED_EDGE('',*,*,#1910,.F.);
#2636=ORIENTED_EDGE('',*,*,#1941,.F.);
#2637=ORIENTED_EDGE('',*,*,#1939,.T.);
#2638=ORIENTED_EDGE('',*,*,#1911,.F.);
#2639=ORIENTED_EDGE('',*,*,#1938,.T.);
#2640=ORIENTED_EDGE('',*,*,#1936,.F.);
#2641=ORIENTED_EDGE('',*,*,#1912,.F.);
#2642=ORIENTED_EDGE('',*,*,#1935,.F.);
#2643=ORIENTED_EDGE('',*,*,#1951,.T.);
#2644=ORIENTED_EDGE('',*,*,#1913,.F.);
#2645=ORIENTED_EDGE('',*,*,#1950,.T.);
#2646=ORIENTED_EDGE('',*,*,#1948,.T.);
#2647=ORIENTED_EDGE('',*,*,#1914,.F.);
#2648=ORIENTED_EDGE('',*,*,#1952,.F.);
#2649=ORIENTED_EDGE('',*,*,#1953,.T.);
#2650=ORIENTED_EDGE('',*,*,#1954,.T.);
#2651=ORIENTED_EDGE('',*,*,#1955,.T.);
#2652=ORIENTED_EDGE('',*,*,#1953,.F.);
#2653=ORIENTED_EDGE('',*,*,#1956,.T.);
#2654=ORIENTED_EDGE('',*,*,#1957,.T.);
#2655=ORIENTED_EDGE('',*,*,#1954,.F.);
#2656=ORIENTED_EDGE('',*,*,#1955,.F.);
#2657=ORIENTED_EDGE('',*,*,#1957,.F.);
#2658=ORIENTED_EDGE('',*,*,#1958,.T.);
#2659=ORIENTED_EDGE('',*,*,#1959,.T.);
#2660=ORIENTED_EDGE('',*,*,#1960,.T.);
#2661=ORIENTED_EDGE('',*,*,#1961,.T.);
#2662=ORIENTED_EDGE('',*,*,#1960,.F.);
#2663=ORIENTED_EDGE('',*,*,#1962,.T.);
#2664=ORIENTED_EDGE('',*,*,#1963,.T.);
#2665=ORIENTED_EDGE('',*,*,#1964,.T.);
#2666=ORIENTED_EDGE('',*,*,#1965,.T.);
#2667=ORIENTED_EDGE('',*,*,#1966,.T.);
#2668=ORIENTED_EDGE('',*,*,#1967,.T.);
#2669=ORIENTED_EDGE('',*,*,#1968,.T.);
#2670=ORIENTED_EDGE('',*,*,#1969,.T.);
#2671=ORIENTED_EDGE('',*,*,#1970,.T.);
#2672=ORIENTED_EDGE('',*,*,#1971,.T.);
#2673=ORIENTED_EDGE('',*,*,#1963,.F.);
#2674=ORIENTED_EDGE('',*,*,#1972,.T.);
#2675=ORIENTED_EDGE('',*,*,#1962,.F.);
#2676=ORIENTED_EDGE('',*,*,#1973,.T.);
#2677=ORIENTED_EDGE('',*,*,#1974,.T.);
#2678=ORIENTED_EDGE('',*,*,#1973,.F.);
#2679=ORIENTED_EDGE('',*,*,#1972,.F.);
#2680=ORIENTED_EDGE('',*,*,#1956,.F.);
#2681=ORIENTED_EDGE('',*,*,#1975,.T.);
#2682=ORIENTED_EDGE('',*,*,#1959,.F.);
#2683=ORIENTED_EDGE('',*,*,#1975,.F.);
#2684=ORIENTED_EDGE('',*,*,#1958,.F.);
#2685=ORIENTED_EDGE('',*,*,#1976,.F.);
#2686=ORIENTED_EDGE('',*,*,#1977,.T.);
#2687=ORIENTED_EDGE('',*,*,#1978,.T.);
#2688=ORIENTED_EDGE('',*,*,#1979,.T.);
#2689=ORIENTED_EDGE('',*,*,#1980,.T.);
#2690=ORIENTED_EDGE('',*,*,#1981,.F.);
#2691=ORIENTED_EDGE('',*,*,#1982,.T.);
#2692=ORIENTED_EDGE('',*,*,#1976,.T.);
#2693=ORIENTED_EDGE('',*,*,#1983,.T.);
#2694=ORIENTED_EDGE('',*,*,#1984,.T.);
#2695=ORIENTED_EDGE('',*,*,#1985,.F.);
#2696=ORIENTED_EDGE('',*,*,#1986,.T.);
#2697=ORIENTED_EDGE('',*,*,#1981,.T.);
#2698=ORIENTED_EDGE('',*,*,#1987,.F.);
#2699=ORIENTED_EDGE('',*,*,#1988,.F.);
#2700=ORIENTED_EDGE('',*,*,#1989,.F.);
#2701=ORIENTED_EDGE('',*,*,#1990,.T.);
#2702=ORIENTED_EDGE('',*,*,#1985,.T.);
#2703=ORIENTED_EDGE('',*,*,#1991,.T.);
#2704=ORIENTED_EDGE('',*,*,#1992,.T.);
#2705=ORIENTED_EDGE('',*,*,#1993,.F.);
#2706=ORIENTED_EDGE('',*,*,#1994,.T.);
#2707=ORIENTED_EDGE('',*,*,#1989,.T.);
#2708=ORIENTED_EDGE('',*,*,#1995,.T.);
#2709=ORIENTED_EDGE('',*,*,#1996,.T.);
#2710=ORIENTED_EDGE('',*,*,#1978,.F.);
#2711=ORIENTED_EDGE('',*,*,#1997,.T.);
#2712=ORIENTED_EDGE('',*,*,#1993,.T.);
#2713=ORIENTED_EDGE('',*,*,#1998,.T.);
#2714=ORIENTED_EDGE('',*,*,#1999,.T.);
#2715=ORIENTED_EDGE('',*,*,#2000,.F.);
#2716=ORIENTED_EDGE('',*,*,#2001,.F.);
#2717=ORIENTED_EDGE('',*,*,#2002,.F.);
#2718=ORIENTED_EDGE('',*,*,#2003,.F.);
#2719=ORIENTED_EDGE('',*,*,#2004,.T.);
#2720=ORIENTED_EDGE('',*,*,#2005,.F.);
#2721=ORIENTED_EDGE('',*,*,#1961,.F.);
#2722=ORIENTED_EDGE('',*,*,#1974,.F.);
#2723=ORIENTED_EDGE('',*,*,#1952,.T.);
#2724=ORIENTED_EDGE('',*,*,#2001,.T.);
#2725=ORIENTED_EDGE('',*,*,#1998,.F.);
#2726=ORIENTED_EDGE('',*,*,#1996,.F.);
#2727=ORIENTED_EDGE('',*,*,#2002,.T.);
#2728=ORIENTED_EDGE('',*,*,#1995,.F.);
#2729=ORIENTED_EDGE('',*,*,#1992,.F.);
#2730=ORIENTED_EDGE('',*,*,#1988,.T.);
#2731=ORIENTED_EDGE('',*,*,#2003,.T.);
#2732=ORIENTED_EDGE('',*,*,#1991,.F.);
#2733=ORIENTED_EDGE('',*,*,#2004,.F.);
#2734=ORIENTED_EDGE('',*,*,#1987,.T.);
#2735=ORIENTED_EDGE('',*,*,#1984,.F.);
#2736=ORIENTED_EDGE('',*,*,#2005,.T.);
#2737=ORIENTED_EDGE('',*,*,#1983,.F.);
#2738=ORIENTED_EDGE('',*,*,#1980,.F.);
#2739=ORIENTED_EDGE('',*,*,#1999,.F.);
#2740=ORIENTED_EDGE('',*,*,#2000,.T.);
#2741=ORIENTED_EDGE('',*,*,#1979,.F.);
#2742=ORIENTED_EDGE('',*,*,#2006,.F.);
#2743=ORIENTED_EDGE('',*,*,#1966,.F.);
#2744=ORIENTED_EDGE('',*,*,#2007,.F.);
#2745=ORIENTED_EDGE('',*,*,#1994,.F.);
#2746=ORIENTED_EDGE('',*,*,#2007,.T.);
#2747=ORIENTED_EDGE('',*,*,#1965,.F.);
#2748=ORIENTED_EDGE('',*,*,#2008,.F.);
#2749=ORIENTED_EDGE('',*,*,#1990,.F.);
#2750=ORIENTED_EDGE('',*,*,#2006,.T.);
#2751=ORIENTED_EDGE('',*,*,#1997,.F.);
#2752=ORIENTED_EDGE('',*,*,#2009,.F.);
#2753=ORIENTED_EDGE('',*,*,#1968,.F.);
#2754=ORIENTED_EDGE('',*,*,#1967,.F.);
#2755=ORIENTED_EDGE('',*,*,#2008,.T.);
#2756=ORIENTED_EDGE('',*,*,#1964,.F.);
#2757=ORIENTED_EDGE('',*,*,#1971,.F.);
#2758=ORIENTED_EDGE('',*,*,#2010,.F.);
#2759=ORIENTED_EDGE('',*,*,#1986,.F.);
#2760=ORIENTED_EDGE('',*,*,#2009,.T.);
#2761=ORIENTED_EDGE('',*,*,#1977,.F.);
#2762=ORIENTED_EDGE('',*,*,#2011,.F.);
#2763=ORIENTED_EDGE('',*,*,#1969,.F.);
#2764=ORIENTED_EDGE('',*,*,#2010,.T.);
#2765=ORIENTED_EDGE('',*,*,#1970,.F.);
#2766=ORIENTED_EDGE('',*,*,#2011,.T.);
#2767=ORIENTED_EDGE('',*,*,#1982,.F.);
#2768=CYLINDRICAL_SURFACE('',#3048,60.);
#2769=CYLINDRICAL_SURFACE('',#3051,60.);
#2770=CYLINDRICAL_SURFACE('',#3054,2.64999999999999);
#2771=CYLINDRICAL_SURFACE('',#3057,2.64999999999999);
#2772=CYLINDRICAL_SURFACE('',#3060,2.64999999999999);
#2773=CYLINDRICAL_SURFACE('',#3063,2.64999999999999);
#2774=CYLINDRICAL_SURFACE('',#3066,2.64999999999999);
#2775=CYLINDRICAL_SURFACE('',#3069,2.64999999999999);
#2776=CYLINDRICAL_SURFACE('',#3072,2.64999999999999);
#2777=CYLINDRICAL_SURFACE('',#3075,2.64999999999999);
#2778=CYLINDRICAL_SURFACE('',#3078,2.64999999999999);
#2779=CYLINDRICAL_SURFACE('',#3081,2.64999999999999);
#2780=CYLINDRICAL_SURFACE('',#3104,60.);
#2781=CYLINDRICAL_SURFACE('',#3105,60.);
#2782=CYLINDRICAL_SURFACE('',#3109,2.64999999999999);
#2783=CYLINDRICAL_SURFACE('',#3112,2.64999999999999);
#2784=CYLINDRICAL_SURFACE('',#3115,2.64999999999999);
#2785=CYLINDRICAL_SURFACE('',#3118,2.64999999999999);
#2786=CYLINDRICAL_SURFACE('',#3121,2.64999999999999);
#2787=CYLINDRICAL_SURFACE('',#3157,10.);
#2788=CYLINDRICAL_SURFACE('',#3191,13.5);
#2789=CYLINDRICAL_SURFACE('',#3196,12.775);
#2790=CYLINDRICAL_SURFACE('',#3200,12.45);
#2791=CYLINDRICAL_SURFACE('',#3212,10.);
#2792=CYLINDRICAL_SURFACE('',#3217,11.05);
#2793=CYLINDRICAL_SURFACE('',#3219,10.725);
#2794=CYLINDRICAL_SURFACE('',#3230,13.5);
#2795=CYLINDRICAL_SURFACE('',#3233,13.5);
#2796=CYLINDRICAL_SURFACE('',#3236,22.5);
#2797=CYLINDRICAL_SURFACE('',#3239,10.5);
#2798=CYLINDRICAL_SURFACE('',#3263,4.25);
#2799=CYLINDRICAL_SURFACE('',#3265,2.5);
#2800=CYLINDRICAL_SURFACE('',#3285,2.5);
#2801=CYLINDRICAL_SURFACE('',#3301,2.1);
#2802=ADVANCED_FACE('',(#442),#2768,.F.);
#2803=ADVANCED_FACE('',(#443),#2769,.F.);
#2804=ADVANCED_FACE('',(#444),#2770,.F.);
#2805=ADVANCED_FACE('',(#445),#2771,.F.);
#2806=ADVANCED_FACE('',(#446),#2772,.F.);
#2807=ADVANCED_FACE('',(#447),#2773,.F.);
#2808=ADVANCED_FACE('',(#448),#2774,.F.);
#2809=ADVANCED_FACE('',(#449),#2775,.F.);
#2810=ADVANCED_FACE('',(#450),#2776,.F.);
#2811=ADVANCED_FACE('',(#451),#2777,.F.);
#2812=ADVANCED_FACE('',(#452),#2778,.F.);
#2813=ADVANCED_FACE('',(#453),#2779,.F.);
#2814=ADVANCED_FACE('',(#454),#343,.F.);
#2815=ADVANCED_FACE('',(#455,#285,#286,#287,#288,#289),#344,.F.);
#2816=ADVANCED_FACE('',(#456,#290,#291,#292,#293,#294),#345,.F.);
#2817=ADVANCED_FACE('',(#457),#346,.T.);
#2818=ADVANCED_FACE('',(#458,#295,#296,#297,#298,#299,#300,#301,#302,#303,
#304),#347,.T.);
#2819=ADVANCED_FACE('',(#459),#348,.T.);
#2820=ADVANCED_FACE('',(#460),#349,.F.);
#2821=ADVANCED_FACE('',(#461),#350,.T.);
#2822=ADVANCED_FACE('',(#462,#305),#351,.F.);
#2823=ADVANCED_FACE('',(#463,#306),#352,.T.);
#2824=ADVANCED_FACE('',(#464),#353,.F.);
#2825=ADVANCED_FACE('',(#465,#307),#354,.F.);
#2826=ADVANCED_FACE('',(#466,#308),#355,.T.);
#2827=ADVANCED_FACE('',(#467),#356,.F.);
#2828=ADVANCED_FACE('',(#468),#357,.F.);
#2829=ADVANCED_FACE('',(#469),#358,.F.);
#2830=ADVANCED_FACE('',(#470),#2780,.F.);
#2831=ADVANCED_FACE('',(#471),#2781,.F.);
#2832=ADVANCED_FACE('',(#472),#359,.F.);
#2833=ADVANCED_FACE('',(#473),#360,.F.);
#2834=ADVANCED_FACE('',(#474),#2782,.F.);
#2835=ADVANCED_FACE('',(#475),#2783,.F.);
#2836=ADVANCED_FACE('',(#476),#2784,.F.);
#2837=ADVANCED_FACE('',(#477),#2785,.F.);
#2838=ADVANCED_FACE('',(#478),#2786,.F.);
#2839=ADVANCED_FACE('',(#479),#361,.F.);
#2840=ADVANCED_FACE('',(#480),#362,.F.);
#2841=ADVANCED_FACE('',(#481),#363,.F.);
#2842=ADVANCED_FACE('',(#482),#364,.F.);
#2843=ADVANCED_FACE('',(#483),#365,.F.);
#2844=ADVANCED_FACE('',(#484),#366,.F.);
#2845=ADVANCED_FACE('',(#485),#367,.F.);
#2846=ADVANCED_FACE('',(#486),#368,.F.);
#2847=ADVANCED_FACE('',(#487),#369,.F.);
#2848=ADVANCED_FACE('',(#488),#370,.F.);
#2849=ADVANCED_FACE('',(#489),#371,.F.);
#2850=ADVANCED_FACE('',(#490),#372,.F.);
#2851=ADVANCED_FACE('',(#491),#373,.F.);
#2852=ADVANCED_FACE('',(#492),#374,.F.);
#2853=ADVANCED_FACE('',(#493),#375,.F.);
#2854=ADVANCED_FACE('',(#494),#376,.F.);
#2855=ADVANCED_FACE('',(#495),#377,.F.);
#2856=ADVANCED_FACE('',(#496),#378,.F.);
#2857=ADVANCED_FACE('',(#497),#379,.F.);
#2858=ADVANCED_FACE('',(#498,#309,#310,#311,#312,#313,#314),#380,.F.);
#2859=ADVANCED_FACE('',(#499,#315,#316,#317,#318,#319,#320),#381,.T.);
#2860=ADVANCED_FACE('',(#500),#382,.T.);
#2861=ADVANCED_FACE('',(#501,#321,#322,#323,#324,#325),#383,.F.);
#2862=ADVANCED_FACE('',(#502,#326,#327,#328,#329,#330),#384,.T.);
#2863=ADVANCED_FACE('',(#503),#385,.F.);
#2864=ADVANCED_FACE('',(#504),#386,.F.);
#2865=ADVANCED_FACE('',(#505),#387,.F.);
#2866=ADVANCED_FACE('',(#506),#388,.F.);
#2867=ADVANCED_FACE('',(#507),#389,.F.);
#2868=ADVANCED_FACE('',(#508),#390,.F.);
#2869=ADVANCED_FACE('',(#509),#391,.F.);
#2870=ADVANCED_FACE('',(#510),#392,.F.);
#2871=ADVANCED_FACE('',(#511),#2787,.T.);
#2872=ADVANCED_FACE('',(#512),#393,.T.);
#2873=ADVANCED_FACE('',(#513),#394,.T.);
#2874=ADVANCED_FACE('',(#514),#395,.T.);
#2875=ADVANCED_FACE('',(#515),#396,.T.);
#2876=ADVANCED_FACE('',(#516),#397,.F.);
#2877=ADVANCED_FACE('',(#517),#398,.F.);
#2878=ADVANCED_FACE('',(#518),#399,.F.);
#2879=ADVANCED_FACE('',(#519),#400,.F.);
#2880=ADVANCED_FACE('',(#520),#401,.F.);
#2881=ADVANCED_FACE('',(#521),#402,.F.);
#2882=ADVANCED_FACE('',(#522),#403,.F.);
#2883=ADVANCED_FACE('',(#523),#404,.F.);
#2884=ADVANCED_FACE('',(#524),#405,.F.);
#2885=ADVANCED_FACE('',(#525),#406,.F.);
#2886=ADVANCED_FACE('',(#526),#407,.F.);
#2887=ADVANCED_FACE('',(#527),#408,.F.);
#2888=ADVANCED_FACE('',(#528),#409,.F.);
#2889=ADVANCED_FACE('',(#529),#410,.T.);
#2890=ADVANCED_FACE('',(#530),#248,.T.);
#2891=ADVANCED_FACE('',(#531),#2788,.T.);
#2892=ADVANCED_FACE('',(#532),#249,.T.);
#2893=ADVANCED_FACE('',(#533),#2789,.F.);
#2894=ADVANCED_FACE('',(#534),#2790,.F.);
#2895=ADVANCED_FACE('',(#535),#250,.T.);
#2896=ADVANCED_FACE('',(#536),#251,.T.);
#2897=ADVANCED_FACE('',(#537),#2791,.F.);
#2898=ADVANCED_FACE('',(#538),#252,.T.);
#2899=ADVANCED_FACE('',(#539),#2792,.T.);
#2900=ADVANCED_FACE('',(#540),#2793,.T.);
#2901=ADVANCED_FACE('',(#541),#253,.T.);
#2902=ADVANCED_FACE('',(#542,#331),#411,.T.);
#2903=ADVANCED_FACE('',(#543,#332),#412,.T.);
#2904=ADVANCED_FACE('',(#544,#333),#413,.T.);
#2905=ADVANCED_FACE('',(#545,#334),#414,.T.);
#2906=ADVANCED_FACE('',(#546),#2794,.F.);
#2907=ADVANCED_FACE('',(#547),#2795,.F.);
#2908=ADVANCED_FACE('',(#548),#2796,.T.);
#2909=ADVANCED_FACE('',(#549),#2797,.F.);
#2910=ADVANCED_FACE('',(#550,#335),#415,.T.);
#2911=ADVANCED_FACE('',(#551,#336),#416,.F.);
#2912=ADVANCED_FACE('',(#552,#337),#417,.T.);
#2913=ADVANCED_FACE('',(#553,#338),#418,.T.);
#2914=ADVANCED_FACE('',(#554),#237,.F.);
#2915=ADVANCED_FACE('',(#555),#254,.T.);
#2916=ADVANCED_FACE('',(#556),#255,.F.);
#2917=ADVANCED_FACE('',(#557),#2798,.T.);
#2918=ADVANCED_FACE('',(#558),#2799,.T.);
#2919=ADVANCED_FACE('',(#559),#238,.T.);
#2920=ADVANCED_FACE('',(#560,#339),#419,.T.);
#2921=ADVANCED_FACE('',(#561),#420,.T.);
#2922=ADVANCED_FACE('',(#562,#340),#421,.T.);
#2923=ADVANCED_FACE('',(#563),#422,.T.);
#2924=ADVANCED_FACE('',(#564),#423,.F.);
#2925=ADVANCED_FACE('',(#565),#424,.T.);
#2926=ADVANCED_FACE('',(#566),#425,.T.);
#2927=ADVANCED_FACE('',(#567),#426,.F.);
#2928=ADVANCED_FACE('',(#568),#427,.F.);
#2929=ADVANCED_FACE('',(#569),#428,.F.);
#2930=ADVANCED_FACE('',(#570),#429,.F.);
#2931=ADVANCED_FACE('',(#571),#430,.F.);
#2932=ADVANCED_FACE('',(#572),#431,.F.);
#2933=ADVANCED_FACE('',(#573),#432,.F.);
#2934=ADVANCED_FACE('',(#574),#433,.F.);
#2935=ADVANCED_FACE('',(#575),#2800,.F.);
#2936=ADVANCED_FACE('',(#576),#239,.F.);
#2937=ADVANCED_FACE('',(#577),#240,.F.);
#2938=ADVANCED_FACE('',(#578),#241,.T.);
#2939=ADVANCED_FACE('',(#579),#256,.T.);
#2940=ADVANCED_FACE('',(#580),#2801,.F.);
#2941=ADVANCED_FACE('',(#581),#434,.T.);
#2942=ADVANCED_FACE('',(#582),#435,.T.);
#2943=ADVANCED_FACE('',(#583),#436,.F.);
#2944=ADVANCED_FACE('',(#584),#437,.T.);
#2945=ADVANCED_FACE('',(#585),#438,.T.);
#2946=ADVANCED_FACE('',(#586),#439,.T.);
#2947=ADVANCED_FACE('',(#587,#341),#440,.F.);
#2948=ADVANCED_FACE('',(#588,#342),#441,.T.);
#2949=ADVANCED_FACE('',(#589),#242,.T.);
#2950=ADVANCED_FACE('',(#590),#243,.T.);
#2951=ADVANCED_FACE('',(#591),#244,.T.);
#2952=ADVANCED_FACE('',(#592),#245,.T.);
#2953=ADVANCED_FACE('',(#593),#246,.T.);
#2954=ADVANCED_FACE('',(#594),#247,.T.);
#2955=ADVANCED_FACE('',(#595),#199,.F.);
#2956=ADVANCED_FACE('',(#596),#200,.F.);
#2957=ADVANCED_FACE('',(#597),#201,.F.);
#2958=ADVANCED_FACE('',(#598),#202,.F.);
#2959=ADVANCED_FACE('',(#599),#203,.F.);
#2960=ADVANCED_FACE('',(#600),#204,.F.);
#2961=CLOSED_SHELL('',(#2802,#2803,#2804,#2805,#2806,#2807,#2808,#2809,
#2810,#2811,#2812,#2813,#2814,#2815,#2816,#2817,#2818,#2819,#2820,#2821,
#2822,#2823,#2824,#2825,#2826,#2827,#2828,#2829,#2830,#2831,#2832,#2833));
#2962=CLOSED_SHELL('',(#2834,#2835,#2836,#2837,#2838,#2839,#2840,#2841,
#2842,#2843,#2844,#2845,#2846,#2847,#2848,#2849,#2850,#2851,#2852,#2853,
#2854,#2855,#2856,#2857,#2858,#2859,#2860,#2861,#2862,#2863,#2864,#2865,
#2866,#2867,#2868,#2869,#2870));
#2963=CLOSED_SHELL('',(#2871,#2872,#2873,#2874,#2875,#2876,#2877,#2878,
#2879,#2880,#2881,#2882,#2883,#2884,#2885,#2886,#2887,#2888,#2889));
#2964=CLOSED_SHELL('',(#2890,#2891,#2892,#2893,#2894,#2895,#2896,#2897,
#2898,#2899,#2900,#2901,#2902,#2903,#2904,#2905));
#2965=CLOSED_SHELL('',(#2906,#2907,#2908,#2909,#2910,#2911,#2912,#2913));
#2966=CLOSED_SHELL('',(#2914,#2915,#2916,#2917,#2918,#2919,#2920,#2921,
#2922,#2923,#2924,#2925,#2926,#2927,#2928,#2929,#2930,#2931,#2932,#2933,
#2934));
#2967=CLOSED_SHELL('',(#2935,#2936,#2937,#2938,#2939,#2940,#2941,#2942,
#2943,#2944,#2945,#2946,#2947,#2948,#2949,#2950,#2951,#2952,#2953,#2954,
#2955,#2956,#2957,#2958,#2959,#2960));
#2968=DERIVED_UNIT_ELEMENT(#2982,1.);
#2969=DERIVED_UNIT_ELEMENT(#5691,-3.);
#2970=DERIVED_UNIT_ELEMENT(#2982,1.);
#2971=DERIVED_UNIT_ELEMENT(#5691,-3.);
#2972=DERIVED_UNIT_ELEMENT(#2982,1.);
#2973=DERIVED_UNIT_ELEMENT(#5691,-3.);
#2974=DERIVED_UNIT_ELEMENT(#2982,1.);
#2975=DERIVED_UNIT_ELEMENT(#5691,-3.);
#2976=DERIVED_UNIT_ELEMENT(#2982,1.);
#2977=DERIVED_UNIT_ELEMENT(#5691,-3.);
#2978=DERIVED_UNIT_ELEMENT(#2982,1.);
#2979=DERIVED_UNIT_ELEMENT(#5691,-3.);
#2980=DERIVED_UNIT_ELEMENT(#2982,1.);
#2981=DERIVED_UNIT_ELEMENT(#5691,-3.);
#2982=(
MASS_UNIT()
NAMED_UNIT(*)
SI_UNIT(.KILO.,.GRAM.)
);
#2983=DERIVED_UNIT((#2968,#2969));
#2984=DERIVED_UNIT((#2970,#2971));
#2985=DERIVED_UNIT((#2972,#2973));
#2986=DERIVED_UNIT((#2974,#2975));
#2987=DERIVED_UNIT((#2976,#2977));
#2988=DERIVED_UNIT((#2978,#2979));
#2989=DERIVED_UNIT((#2980,#2981));
#2990=MEASURE_REPRESENTATION_ITEM('density measure',
POSITIVE_RATIO_MEASURE(7850.),#2983);
#2991=MEASURE_REPRESENTATION_ITEM('density measure',
POSITIVE_RATIO_MEASURE(7850.),#2984);
#2992=MEASURE_REPRESENTATION_ITEM('density measure',
POSITIVE_RATIO_MEASURE(7850.),#2985);
#2993=MEASURE_REPRESENTATION_ITEM('density measure',
POSITIVE_RATIO_MEASURE(7850.),#2986);
#2994=MEASURE_REPRESENTATION_ITEM('density measure',
POSITIVE_RATIO_MEASURE(7850.),#2987);
#2995=MEASURE_REPRESENTATION_ITEM('density measure',
POSITIVE_RATIO_MEASURE(7850.),#2988);
#2996=MEASURE_REPRESENTATION_ITEM('density measure',
POSITIVE_RATIO_MEASURE(7850.),#2989);
#2997=PROPERTY_DEFINITION_REPRESENTATION(#3032,#3011);
#2998=PROPERTY_DEFINITION_REPRESENTATION(#3033,#3012);
#2999=PROPERTY_DEFINITION_REPRESENTATION(#3034,#3013);
#3000=PROPERTY_DEFINITION_REPRESENTATION(#3035,#3014);
#3001=PROPERTY_DEFINITION_REPRESENTATION(#3036,#3015);
#3002=PROPERTY_DEFINITION_REPRESENTATION(#3037,#3016);
#3003=PROPERTY_DEFINITION_REPRESENTATION(#3038,#3017);
#3004=PROPERTY_DEFINITION_REPRESENTATION(#3039,#3018);
#3005=PROPERTY_DEFINITION_REPRESENTATION(#3040,#3019);
#3006=PROPERTY_DEFINITION_REPRESENTATION(#3041,#3020);
#3007=PROPERTY_DEFINITION_REPRESENTATION(#3042,#3021);
#3008=PROPERTY_DEFINITION_REPRESENTATION(#3043,#3022);
#3009=PROPERTY_DEFINITION_REPRESENTATION(#3044,#3023);
#3010=PROPERTY_DEFINITION_REPRESENTATION(#3045,#3024);
#3011=REPRESENTATION('material name',(#3025),#5682);
#3012=REPRESENTATION('density',(#2990),#5682);
#3013=REPRESENTATION('material name',(#3026),#5683);
#3014=REPRESENTATION('density',(#2991),#5683);
#3015=REPRESENTATION('material name',(#3027),#5684);
#3016=REPRESENTATION('density',(#2992),#5684);
#3017=REPRESENTATION('material name',(#3028),#5685);
#3018=REPRESENTATION('density',(#2993),#5685);
#3019=REPRESENTATION('material name',(#3029),#5686);
#3020=REPRESENTATION('density',(#2994),#5686);
#3021=REPRESENTATION('material name',(#3030),#5687);
#3022=REPRESENTATION('density',(#2995),#5687);
#3023=REPRESENTATION('material name',(#3031),#5688);
#3024=REPRESENTATION('density',(#2996),#5688);
#3025=DESCRIPTIVE_REPRESENTATION_ITEM('Steel','Steel');
#3026=DESCRIPTIVE_REPRESENTATION_ITEM('Steel','Steel');
#3027=DESCRIPTIVE_REPRESENTATION_ITEM('Steel','Steel');
#3028=DESCRIPTIVE_REPRESENTATION_ITEM('Steel','Steel');
#3029=DESCRIPTIVE_REPRESENTATION_ITEM('Steel','Steel');
#3030=DESCRIPTIVE_REPRESENTATION_ITEM('Steel','Steel');
#3031=DESCRIPTIVE_REPRESENTATION_ITEM('Steel','Steel');
#3032=PROPERTY_DEFINITION('material property','material name',#5767);
#3033=PROPERTY_DEFINITION('material property','density of part',#5767);
#3034=PROPERTY_DEFINITION('material property','material name',#5768);
#3035=PROPERTY_DEFINITION('material property','density of part',#5768);
#3036=PROPERTY_DEFINITION('material property','material name',#5769);
#3037=PROPERTY_DEFINITION('material property','density of part',#5769);
#3038=PROPERTY_DEFINITION('material property','material name',#5770);
#3039=PROPERTY_DEFINITION('material property','density of part',#5770);
#3040=PROPERTY_DEFINITION('material property','material name',#5771);
#3041=PROPERTY_DEFINITION('material property','density of part',#5771);
#3042=PROPERTY_DEFINITION('material property','material name',#5772);
#3043=PROPERTY_DEFINITION('material property','density of part',#5772);
#3044=PROPERTY_DEFINITION('material property','material name',#5773);
#3045=PROPERTY_DEFINITION('material property','density of part',#5773);
#3046=AXIS2_PLACEMENT_3D('',#4246,#3369,#3370);
#3047=AXIS2_PLACEMENT_3D('',#4247,#3371,#3372);
#3048=AXIS2_PLACEMENT_3D('',#4248,#3373,#3374);
#3049=AXIS2_PLACEMENT_3D('',#4251,#3375,#3376);
#3050=AXIS2_PLACEMENT_3D('',#4255,#3378,#3379);
#3051=AXIS2_PLACEMENT_3D('',#4257,#3381,#3382);
#3052=AXIS2_PLACEMENT_3D('',#4260,#3383,#3384);
#3053=AXIS2_PLACEMENT_3D('',#4264,#3386,#3387);
#3054=AXIS2_PLACEMENT_3D('',#4266,#3389,#3390);
#3055=AXIS2_PLACEMENT_3D('',#4268,#3391,#3392);
#3056=AXIS2_PLACEMENT_3D('',#4271,#3394,#3395);
#3057=AXIS2_PLACEMENT_3D('',#4272,#3396,#3397);
#3058=AXIS2_PLACEMENT_3D('',#4274,#3398,#3399);
#3059=AXIS2_PLACEMENT_3D('',#4277,#3401,#3402);
#3060=AXIS2_PLACEMENT_3D('',#4278,#3403,#3404);
#3061=AXIS2_PLACEMENT_3D('',#4280,#3405,#3406);
#3062=AXIS2_PLACEMENT_3D('',#4283,#3408,#3409);
#3063=AXIS2_PLACEMENT_3D('',#4284,#3410,#3411);
#3064=AXIS2_PLACEMENT_3D('',#4286,#3412,#3413);
#3065=AXIS2_PLACEMENT_3D('',#4289,#3415,#3416);
#3066=AXIS2_PLACEMENT_3D('',#4290,#3417,#3418);
#3067=AXIS2_PLACEMENT_3D('',#4292,#3419,#3420);
#3068=AXIS2_PLACEMENT_3D('',#4295,#3422,#3423);
#3069=AXIS2_PLACEMENT_3D('',#4296,#3424,#3425);
#3070=AXIS2_PLACEMENT_3D('',#4298,#3426,#3427);
#3071=AXIS2_PLACEMENT_3D('',#4301,#3429,#3430);
#3072=AXIS2_PLACEMENT_3D('',#4302,#3431,#3432);
#3073=AXIS2_PLACEMENT_3D('',#4304,#3433,#3434);
#3074=AXIS2_PLACEMENT_3D('',#4307,#3436,#3437);
#3075=AXIS2_PLACEMENT_3D('',#4308,#3438,#3439);
#3076=AXIS2_PLACEMENT_3D('',#4310,#3440,#3441);
#3077=AXIS2_PLACEMENT_3D('',#4313,#3443,#3444);
#3078=AXIS2_PLACEMENT_3D('',#4314,#3445,#3446);
#3079=AXIS2_PLACEMENT_3D('',#4316,#3447,#3448);
#3080=AXIS2_PLACEMENT_3D('',#4319,#3450,#3451);
#3081=AXIS2_PLACEMENT_3D('',#4320,#3452,#3453);
#3082=AXIS2_PLACEMENT_3D('',#4322,#3454,#3455);
#3083=AXIS2_PLACEMENT_3D('',#4325,#3457,#3458);
#3084=AXIS2_PLACEMENT_3D('',#4326,#3459,#3460);
#3085=AXIS2_PLACEMENT_3D('',#4335,#3465,#3466);
#3086=AXIS2_PLACEMENT_3D('',#4344,#3471,#3472);
#3087=AXIS2_PLACEMENT_3D('',#4353,#3477,#3478);
#3088=AXIS2_PLACEMENT_3D('',#4369,#3488,#3489);
#3089=AXIS2_PLACEMENT_3D('',#4375,#3493,#3494);
#3090=AXIS2_PLACEMENT_3D('',#4388,#3503,#3504);
#3091=AXIS2_PLACEMENT_3D('',#4389,#3505,#3506);
#3092=AXIS2_PLACEMENT_3D('',#4390,#3507,#3508);
#3093=AXIS2_PLACEMENT_3D('',#4395,#3511,#3512);
#3094=AXIS2_PLACEMENT_3D('',#4397,#3514,#3515);
#3095=AXIS2_PLACEMENT_3D('',#4401,#3517,#3518);
#3096=AXIS2_PLACEMENT_3D('',#4404,#3521,#3522);
#3097=AXIS2_PLACEMENT_3D('',#4405,#3523,#3524);
#3098=AXIS2_PLACEMENT_3D('',#4410,#3527,#3528);
#3099=AXIS2_PLACEMENT_3D('',#4412,#3530,#3531);
#3100=AXIS2_PLACEMENT_3D('',#4416,#3533,#3534);
#3101=AXIS2_PLACEMENT_3D('',#4419,#3537,#3538);
#3102=AXIS2_PLACEMENT_3D('',#4420,#3539,#3540);
#3103=AXIS2_PLACEMENT_3D('',#4422,#3542,#3543);
#3104=AXIS2_PLACEMENT_3D('',#4424,#3545,#3546);
#3105=AXIS2_PLACEMENT_3D('',#4425,#3547,#3548);
#3106=AXIS2_PLACEMENT_3D('',#4428,#3551,#3552);
#3107=AXIS2_PLACEMENT_3D('',#4429,#3553,#3554);
#3108=AXIS2_PLACEMENT_3D('',#4430,#3555,#3556);
#3109=AXIS2_PLACEMENT_3D('',#4431,#3557,#3558);
#3110=AXIS2_PLACEMENT_3D('',#4433,#3559,#3560);
#3111=AXIS2_PLACEMENT_3D('',#4436,#3562,#3563);
#3112=AXIS2_PLACEMENT_3D('',#4437,#3564,#3565);
#3113=AXIS2_PLACEMENT_3D('',#4439,#3566,#3567);
#3114=AXIS2_PLACEMENT_3D('',#4442,#3569,#3570);
#3115=AXIS2_PLACEMENT_3D('',#4443,#3571,#3572);
#3116=AXIS2_PLACEMENT_3D('',#4445,#3573,#3574);
#3117=AXIS2_PLACEMENT_3D('',#4448,#3576,#3577);
#3118=AXIS2_PLACEMENT_3D('',#4449,#3578,#3579);
#3119=AXIS2_PLACEMENT_3D('',#4451,#3580,#3581);
#3120=AXIS2_PLACEMENT_3D('',#4454,#3583,#3584);
#3121=AXIS2_PLACEMENT_3D('',#4455,#3585,#3586);
#3122=AXIS2_PLACEMENT_3D('',#4457,#3587,#3588);
#3123=AXIS2_PLACEMENT_3D('',#4460,#3590,#3591);
#3124=AXIS2_PLACEMENT_3D('',#4461,#3592,#3593);
#3125=AXIS2_PLACEMENT_3D('',#4470,#3598,#3599);
#3126=AXIS2_PLACEMENT_3D('',#4476,#3603,#3604);
#3127=AXIS2_PLACEMENT_3D('',#4482,#3608,#3609);
#3128=AXIS2_PLACEMENT_3D('',#4485,#3612,#3613);
#3129=AXIS2_PLACEMENT_3D('',#4494,#3618,#3619);
#3130=AXIS2_PLACEMENT_3D('',#4500,#3623,#3624);
#3131=AXIS2_PLACEMENT_3D('',#4506,#3628,#3629);
#3132=AXIS2_PLACEMENT_3D('',#4509,#3632,#3633);
#3133=AXIS2_PLACEMENT_3D('',#4518,#3638,#3639);
#3134=AXIS2_PLACEMENT_3D('',#4524,#3643,#3644);
#3135=AXIS2_PLACEMENT_3D('',#4530,#3648,#3649);
#3136=AXIS2_PLACEMENT_3D('',#4533,#3652,#3653);
#3137=AXIS2_PLACEMENT_3D('',#4542,#3658,#3659);
#3138=AXIS2_PLACEMENT_3D('',#4548,#3663,#3664);
#3139=AXIS2_PLACEMENT_3D('',#4554,#3668,#3669);
#3140=AXIS2_PLACEMENT_3D('',#4557,#3672,#3673);
#3141=AXIS2_PLACEMENT_3D('',#4570,#3680,#3681);
#3142=AXIS2_PLACEMENT_3D('',#4583,#3688,#3689);
#3143=AXIS2_PLACEMENT_3D('',#4586,#3692,#3693);
#3144=AXIS2_PLACEMENT_3D('',#4604,#3703,#3704);
#3145=AXIS2_PLACEMENT_3D('',#4622,#3714,#3715);
#3146=AXIS2_PLACEMENT_3D('',#4625,#3718,#3719);
#3147=AXIS2_PLACEMENT_3D('',#4626,#3720,#3721);
#3148=AXIS2_PLACEMENT_3D('',#4627,#3722,#3723);
#3149=AXIS2_PLACEMENT_3D('',#4630,#3726,#3727);
#3150=AXIS2_PLACEMENT_3D('',#4632,#3729,#3730);
#3151=AXIS2_PLACEMENT_3D('',#4634,#3732,#3733);
#3152=AXIS2_PLACEMENT_3D('',#4635,#3734,#3735);
#3153=AXIS2_PLACEMENT_3D('',#4638,#3738,#3739);
#3154=AXIS2_PLACEMENT_3D('',#4640,#3741,#3742);
#3155=AXIS2_PLACEMENT_3D('',#4642,#3744,#3745);
#3156=AXIS2_PLACEMENT_3D('',#4643,#3746,#3747);
#3157=AXIS2_PLACEMENT_3D('',#4644,#3748,#3749);
#3158=AXIS2_PLACEMENT_3D('',#4647,#3750,#3751);
#3159=AXIS2_PLACEMENT_3D('',#4649,#3752,#3753);
#3160=AXIS2_PLACEMENT_3D('',#4651,#3754,#3755);
#3161=AXIS2_PLACEMENT_3D('',#4655,#3757,#3758);
#3162=AXIS2_PLACEMENT_3D('',#4657,#3759,#3760);
#3163=AXIS2_PLACEMENT_3D('',#4659,#3761,#3762);
#3164=AXIS2_PLACEMENT_3D('',#4661,#3763,#3764);
#3165=AXIS2_PLACEMENT_3D('',#4662,#3765,#3766);
#3166=AXIS2_PLACEMENT_3D('',#4664,#3767,#3768);
#3167=AXIS2_PLACEMENT_3D('',#4665,#3769,#3770);
#3168=AXIS2_PLACEMENT_3D('',#4666,#3771,#3772);
#3169=AXIS2_PLACEMENT_3D('',#4668,#3774,#3775);
#3170=AXIS2_PLACEMENT_3D('',#4670,#3777,#3778);
#3171=AXIS2_PLACEMENT_3D('',#4672,#3780,#3781);
#3172=AXIS2_PLACEMENT_3D('',#4674,#3783,#3784);
#3173=AXIS2_PLACEMENT_3D('',#4676,#3786,#3787);
#3174=AXIS2_PLACEMENT_3D('',#4678,#3789,#3790);
#3175=AXIS2_PLACEMENT_3D('',#4680,#3792,#3793);
#3176=AXIS2_PLACEMENT_3D('',#4682,#3795,#3796);
#3177=AXIS2_PLACEMENT_3D('',#4691,#3801,#3802);
#3178=AXIS2_PLACEMENT_3D('',#4694,#3805,#3806);
#3179=AXIS2_PLACEMENT_3D('',#4696,#3808,#3809);
#3180=AXIS2_PLACEMENT_3D('',#4698,#3811,#3812);
#3181=AXIS2_PLACEMENT_3D('',#4699,#3813,#3814);
#3182=AXIS2_PLACEMENT_3D('',#4705,#3818,#3819);
#3183=AXIS2_PLACEMENT_3D('',#4709,#3822,#3823);
#3184=AXIS2_PLACEMENT_3D('',#4713,#3826,#3827);
#3185=AXIS2_PLACEMENT_3D('',#4715,#3829,#3830);
#3186=AXIS2_PLACEMENT_3D('',#4716,#3831,#3832);
#3187=AXIS2_PLACEMENT_3D('',#4717,#3833,#3834);
#3188=AXIS2_PLACEMENT_3D('',#4719,#3835,#3836);
#3189=AXIS2_PLACEMENT_3D('',#4721,#3837,#3838);
#3190=AXIS2_PLACEMENT_3D('',#4722,#3839,#3840);
#3191=AXIS2_PLACEMENT_3D('',#4723,#3841,#3842);
#3192=AXIS2_PLACEMENT_3D('',#4726,#3844,#3845);
#3193=AXIS2_PLACEMENT_3D('',#4727,#3846,#3847);
#3194=AXIS2_PLACEMENT_3D('',#4729,#3848,#3849);
#3195=AXIS2_PLACEMENT_3D('',#4730,#3850,#3851);
#3196=AXIS2_PLACEMENT_3D('',#4731,#3852,#3853);
#3197=AXIS2_PLACEMENT_3D('',#4733,#3854,#3855);
#3198=AXIS2_PLACEMENT_3D('',#4737,#3857,#3858);
#3199=AXIS2_PLACEMENT_3D('',#4738,#3859,#3860);
#3200=AXIS2_PLACEMENT_3D('',#4739,#3861,#3862);
#3201=AXIS2_PLACEMENT_3D('',#4742,#3863,#3864);
#3202=AXIS2_PLACEMENT_3D('',#4743,#3865,#3866);
#3203=AXIS2_PLACEMENT_3D('',#4746,#3868,#3869);
#3204=AXIS2_PLACEMENT_3D('',#4747,#3870,#3871);
#3205=AXIS2_PLACEMENT_3D('',#4750,#3872,#3873);
#3206=AXIS2_PLACEMENT_3D('',#4751,#3874,#3875);
#3207=AXIS2_PLACEMENT_3D('',#4752,#3876,#3877);
#3208=AXIS2_PLACEMENT_3D('',#4753,#3878,#3879);
#3209=AXIS2_PLACEMENT_3D('',#4755,#3880,#3881);
#3210=AXIS2_PLACEMENT_3D('',#4757,#3882,#3883);
#3211=AXIS2_PLACEMENT_3D('',#4758,#3884,#3885);
#3212=AXIS2_PLACEMENT_3D('',#4759,#3886,#3887);
#3213=AXIS2_PLACEMENT_3D('',#4762,#3889,#3890);
#3214=AXIS2_PLACEMENT_3D('',#4763,#3891,#3892);
#3215=AXIS2_PLACEMENT_3D('',#4765,#3893,#3894);
#3216=AXIS2_PLACEMENT_3D('',#4766,#3895,#3896);
#3217=AXIS2_PLACEMENT_3D('',#4767,#3897,#3898);
#3218=AXIS2_PLACEMENT_3D('',#4770,#3900,#3901);
#3219=AXIS2_PLACEMENT_3D('',#4771,#3902,#3903);
#3220=AXIS2_PLACEMENT_3D('',#4773,#3904,#3905);
#3221=AXIS2_PLACEMENT_3D('',#4777,#3907,#3908);
#3222=AXIS2_PLACEMENT_3D('',#4778,#3909,#3910);
#3223=AXIS2_PLACEMENT_3D('',#4779,#3911,#3912);
#3224=AXIS2_PLACEMENT_3D('',#4780,#3913,#3914);
#3225=AXIS2_PLACEMENT_3D('',#4781,#3915,#3916);
#3226=AXIS2_PLACEMENT_3D('',#4782,#3917,#3918);
#3227=AXIS2_PLACEMENT_3D('',#4783,#3919,#3920);
#3228=AXIS2_PLACEMENT_3D('',#4784,#3921,#3922);
#3229=AXIS2_PLACEMENT_3D('',#4785,#3923,#3924);
#3230=AXIS2_PLACEMENT_3D('',#4786,#3925,#3926);
#3231=AXIS2_PLACEMENT_3D('',#4788,#3927,#3928);
#3232=AXIS2_PLACEMENT_3D('',#4791,#3930,#3931);
#3233=AXIS2_PLACEMENT_3D('',#4792,#3932,#3933);
#3234=AXIS2_PLACEMENT_3D('',#4794,#3934,#3935);
#3235=AXIS2_PLACEMENT_3D('',#4797,#3937,#3938);
#3236=AXIS2_PLACEMENT_3D('',#4798,#3939,#3940);
#3237=AXIS2_PLACEMENT_3D('',#4800,#3941,#3942);
#3238=AXIS2_PLACEMENT_3D('',#4803,#3944,#3945);
#3239=AXIS2_PLACEMENT_3D('',#4804,#3946,#3947);
#3240=AXIS2_PLACEMENT_3D('',#4806,#3948,#3949);
#3241=AXIS2_PLACEMENT_3D('',#4809,#3951,#3952);
#3242=AXIS2_PLACEMENT_3D('',#4810,#3953,#3954);
#3243=AXIS2_PLACEMENT_3D('',#4811,#3955,#3956);
#3244=AXIS2_PLACEMENT_3D('',#4812,#3957,#3958);
#3245=AXIS2_PLACEMENT_3D('',#4813,#3959,#3960);
#3246=AXIS2_PLACEMENT_3D('',#4814,#3961,#3962);
#3247=AXIS2_PLACEMENT_3D('',#4815,#3963,#3964);
#3248=AXIS2_PLACEMENT_3D('',#4820,#3966,#3967);
#3249=AXIS2_PLACEMENT_3D('',#4822,#3968,#3969);
#3250=AXIS2_PLACEMENT_3D('',#4824,#3970,#3971);
#3251=AXIS2_PLACEMENT_3D('',#4826,#3972,#3973);
#3252=AXIS2_PLACEMENT_3D('',#4828,#3974,#3975);
#3253=AXIS2_PLACEMENT_3D('',#4829,#3976,#3977);
#3254=AXIS2_PLACEMENT_3D('',#4830,#3978,#3979);
#3255=AXIS2_PLACEMENT_3D('',#4832,#3980,#3981);
#3256=AXIS2_PLACEMENT_3D('',#4834,#3982,#3983);
#3257=AXIS2_PLACEMENT_3D('',#4835,#3984,#3985);
#3258=AXIS2_PLACEMENT_3D('',#4836,#3986,#3987);
#3259=AXIS2_PLACEMENT_3D('',#4839,#3988,#3989);
#3260=AXIS2_PLACEMENT_3D('',#4840,#3990,#3991);
#3261=AXIS2_PLACEMENT_3D('',#4842,#3992,#3993);
#3262=AXIS2_PLACEMENT_3D('',#4843,#3994,#3995);
#3263=AXIS2_PLACEMENT_3D('',#4844,#3996,#3997);
#3264=AXIS2_PLACEMENT_3D('',#4847,#3999,#4000);
#3265=AXIS2_PLACEMENT_3D('',#4848,#4001,#4002);
#3266=AXIS2_PLACEMENT_3D('',#4851,#4004,#4005);
#3267=AXIS2_PLACEMENT_3D('',#4852,#4006,#4007);
#3268=AXIS2_PLACEMENT_3D('',#4855,#4009,#4010);
#3269=AXIS2_PLACEMENT_3D('',#4856,#4011,#4012);
#3270=AXIS2_PLACEMENT_3D('',#4869,#4019,#4020);
#3271=AXIS2_PLACEMENT_3D('',#4870,#4021,#4022);
#3272=AXIS2_PLACEMENT_3D('',#4871,#4023,#4024);
#3273=AXIS2_PLACEMENT_3D('',#4878,#4029,#4030);
#3274=AXIS2_PLACEMENT_3D('',#4883,#4034,#4035);
#3275=AXIS2_PLACEMENT_3D('',#4888,#4039,#4040);
#3276=AXIS2_PLACEMENT_3D('',#4893,#4044,#4045);
#3277=AXIS2_PLACEMENT_3D('',#4898,#4049,#4050);
#3278=AXIS2_PLACEMENT_3D('',#4901,#4053,#4054);
#3279=AXIS2_PLACEMENT_3D('',#4902,#4055,#4056);
#3280=AXIS2_PLACEMENT_3D('',#4903,#4057,#4058);
#3281=AXIS2_PLACEMENT_3D('',#4904,#4059,#4060);
#3282=AXIS2_PLACEMENT_3D('',#4905,#4061,#4062);
#3283=AXIS2_PLACEMENT_3D('',#4906,#4063,#4064);
#3284=AXIS2_PLACEMENT_3D('',#4907,#4065,#4066);
#3285=AXIS2_PLACEMENT_3D('',#4908,#4067,#4068);
#3286=AXIS2_PLACEMENT_3D('',#4910,#4069,#4070);
#3287=AXIS2_PLACEMENT_3D('',#4914,#4072,#4073);
#3288=AXIS2_PLACEMENT_3D('',#4915,#4074,#4075);
#3289=AXIS2_PLACEMENT_3D('',#4916,#4076,#4077);
#3290=AXIS2_PLACEMENT_3D('',#4919,#4078,#4079);
#3291=AXIS2_PLACEMENT_3D('',#4921,#4081,#4082);
#3292=AXIS2_PLACEMENT_3D('',#4922,#4083,#4084);
#3293=AXIS2_PLACEMENT_3D('',#4924,#4085,#4086);
#3294=AXIS2_PLACEMENT_3D('',#4927,#4088,#4089);
#3295=AXIS2_PLACEMENT_3D('',#4928,#4090,#4091);
#3296=AXIS2_PLACEMENT_3D('',#4931,#4092,#4093);
#3297=AXIS2_PLACEMENT_3D('',#5103,#4095,#4096);
#3298=AXIS2_PLACEMENT_3D('',#5104,#4097,#4098);
#3299=AXIS2_PLACEMENT_3D('',#5106,#4099,#4100);
#3300=AXIS2_PLACEMENT_3D('',#5107,#4101,#4102);
#3301=AXIS2_PLACEMENT_3D('',#5108,#4103,#4104);
#3302=AXIS2_PLACEMENT_3D('',#5110,#4106,#4107);
#3303=AXIS2_PLACEMENT_3D('',#5152,#4110,#4111);
#3304=AXIS2_PLACEMENT_3D('',#5191,#4113,#4114);
#3305=AXIS2_PLACEMENT_3D('',#5230,#4116,#4117);
#3306=AXIS2_PLACEMENT_3D('',#5269,#4119,#4120);
#3307=AXIS2_PLACEMENT_3D('',#5308,#4122,#4123);
#3308=AXIS2_PLACEMENT_3D('',#5344,#4124,#4125);
#3309=AXIS2_PLACEMENT_3D('',#5345,#4126,#4127);
#3310=AXIS2_PLACEMENT_3D('',#5346,#4128,#4129);
#3311=AXIS2_PLACEMENT_3D('',#5347,#4130,#4131);
#3312=AXIS2_PLACEMENT_3D('',#5348,#4132,#4133);
#3313=AXIS2_PLACEMENT_3D('',#5349,#4134,#4135);
#3314=AXIS2_PLACEMENT_3D('',#5350,#4136,#4137);
#3315=AXIS2_PLACEMENT_3D('',#5351,#4138,#4139);
#3316=AXIS2_PLACEMENT_3D('',#5352,#4140,#4141);
#3317=AXIS2_PLACEMENT_3D('',#5353,#4142,#4143);
#3318=AXIS2_PLACEMENT_3D('',#5354,#4144,#4145);
#3319=AXIS2_PLACEMENT_3D('',#5355,#4146,#4147);
#3320=AXIS2_PLACEMENT_3D('',#5356,#4148,#4149);
#3321=AXIS2_PLACEMENT_3D('',#5357,#4150,#4151);
#3322=AXIS2_PLACEMENT_3D('',#5625,#4152,#4153);
#3323=AXIS2_PLACEMENT_3D('',#5626,#4154,#4155);
#3324=AXIS2_PLACEMENT_3D('',#5627,#4156,#4157);
#3325=AXIS2_PLACEMENT_3D('',#5628,#4158,#4159);
#3326=AXIS2_PLACEMENT_3D('',#5629,#4160,#4161);
#3327=AXIS2_PLACEMENT_3D('',#5630,#4162,#4163);
#3328=AXIS2_PLACEMENT_3D('',#5631,#4164,#4165);
#3329=AXIS2_PLACEMENT_3D('',#5632,#4166,#4167);
#3330=AXIS2_PLACEMENT_3D('',#5633,#4168,#4169);
#3331=AXIS2_PLACEMENT_3D('',#5634,#4170,#4171);
#3332=AXIS2_PLACEMENT_3D('',#5635,#4172,#4173);
#3333=AXIS2_PLACEMENT_3D('',#5636,#4174,#4175);
#3334=AXIS2_PLACEMENT_3D('',#5637,#4176,#4177);
#3335=AXIS2_PLACEMENT_3D('',#5638,#4178,#4179);
#3336=AXIS2_PLACEMENT_3D('',#5639,#4180,#4181);
#3337=AXIS2_PLACEMENT_3D('',#5640,#4182,#4183);
#3338=AXIS2_PLACEMENT_3D('',#5641,#4184,#4185);
#3339=AXIS2_PLACEMENT_3D('',#5642,#4186,#4187);
#3340=AXIS2_PLACEMENT_3D('',#5643,#4188,#4189);
#3341=AXIS2_PLACEMENT_3D('',#5644,#4190,#4191);
#3342=AXIS2_PLACEMENT_3D('',#5645,#4192,#4193);
#3343=AXIS2_PLACEMENT_3D('',#5646,#4194,#4195);
#3344=AXIS2_PLACEMENT_3D('',#5647,#4196,#4197);
#3345=AXIS2_PLACEMENT_3D('',#5648,#4198,#4199);
#3346=AXIS2_PLACEMENT_3D('',#5649,#4200,#4201);
#3347=AXIS2_PLACEMENT_3D('',#5650,#4202,#4203);
#3348=AXIS2_PLACEMENT_3D('',#5651,#4204,#4205);
#3349=AXIS2_PLACEMENT_3D('',#5652,#4206,#4207);
#3350=AXIS2_PLACEMENT_3D('',#5653,#4208,#4209);
#3351=AXIS2_PLACEMENT_3D('',#5654,#4210,#4211);
#3352=AXIS2_PLACEMENT_3D('',#5655,#4212,#4213);
#3353=AXIS2_PLACEMENT_3D('',#5656,#4214,#4215);
#3354=AXIS2_PLACEMENT_3D('',#5657,#4216,#4217);
#3355=AXIS2_PLACEMENT_3D('',#5658,#4218,#4219);
#3356=AXIS2_PLACEMENT_3D('',#5659,#4220,#4221);
#3357=AXIS2_PLACEMENT_3D('',#5660,#4222,#4223);
#3358=AXIS2_PLACEMENT_3D('',#5661,#4224,#4225);
#3359=AXIS2_PLACEMENT_3D('',#5662,#4226,#4227);
#3360=AXIS2_PLACEMENT_3D('',#5663,#4228,#4229);
#3361=AXIS2_PLACEMENT_3D('',#5664,#4230,#4231);
#3362=AXIS2_PLACEMENT_3D('',#5665,#4232,#4233);
#3363=AXIS2_PLACEMENT_3D('',#5666,#4234,#4235);
#3364=AXIS2_PLACEMENT_3D('',#5667,#4236,#4237);
#3365=AXIS2_PLACEMENT_3D('',#5668,#4238,#4239);
#3366=AXIS2_PLACEMENT_3D('',#5669,#4240,#4241);
#3367=AXIS2_PLACEMENT_3D('',#5670,#4242,#4243);
#3368=AXIS2_PLACEMENT_3D('',#5671,#4244,#4245);
#3369=DIRECTION('axis',(0.,0.,1.));
#3370=DIRECTION('refdir',(1.,0.,0.));
#3371=DIRECTION('axis',(0.,0.,1.));
#3372=DIRECTION('refdir',(1.,0.,0.));
#3373=DIRECTION('center_axis',(0.,0.,1.));
#3374=DIRECTION('ref_axis',(1.,0.,0.));
#3375=DIRECTION('center_axis',(0.,0.,1.));
#3376=DIRECTION('ref_axis',(1.,0.,0.));
#3377=DIRECTION('',(0.,0.,1.));
#3378=DIRECTION('center_axis',(0.,0.,1.));
#3379=DIRECTION('ref_axis',(1.,0.,0.));
#3380=DIRECTION('',(0.,0.,1.));
#3381=DIRECTION('center_axis',(0.,0.,1.));
#3382=DIRECTION('ref_axis',(1.,0.,0.));
#3383=DIRECTION('center_axis',(0.,0.,1.));
#3384=DIRECTION('ref_axis',(1.,0.,0.));
#3385=DIRECTION('',(0.,0.,1.));
#3386=DIRECTION('center_axis',(0.,0.,1.));
#3387=DIRECTION('ref_axis',(1.,0.,0.));
#3388=DIRECTION('',(0.,0.,1.));
#3389=DIRECTION('center_axis',(0.,1.,0.));
#3390=DIRECTION('ref_axis',(0.,0.,-1.));
#3391=DIRECTION('center_axis',(0.,-1.,0.));
#3392=DIRECTION('ref_axis',(0.,0.,-1.));
#3393=DIRECTION('',(0.,1.,0.));
#3394=DIRECTION('center_axis',(0.,-1.,0.));
#3395=DIRECTION('ref_axis',(0.,0.,-1.));
#3396=DIRECTION('center_axis',(0.,1.,0.));
#3397=DIRECTION('ref_axis',(0.,0.,-1.));
#3398=DIRECTION('center_axis',(0.,-1.,0.));
#3399=DIRECTION('ref_axis',(0.,0.,-1.));
#3400=DIRECTION('',(0.,1.,0.));
#3401=DIRECTION('center_axis',(0.,-1.,0.));
#3402=DIRECTION('ref_axis',(0.,0.,-1.));
#3403=DIRECTION('center_axis',(0.,1.,0.));
#3404=DIRECTION('ref_axis',(0.,0.,-1.));
#3405=DIRECTION('center_axis',(0.,-1.,0.));
#3406=DIRECTION('ref_axis',(0.,0.,-1.));
#3407=DIRECTION('',(0.,1.,0.));
#3408=DIRECTION('center_axis',(0.,-1.,0.));
#3409=DIRECTION('ref_axis',(0.,0.,-1.));
#3410=DIRECTION('center_axis',(0.,1.,0.));
#3411=DIRECTION('ref_axis',(0.,0.,-1.));
#3412=DIRECTION('center_axis',(0.,-1.,0.));
#3413=DIRECTION('ref_axis',(0.,0.,-1.));
#3414=DIRECTION('',(0.,1.,0.));
#3415=DIRECTION('center_axis',(0.,-1.,0.));
#3416=DIRECTION('ref_axis',(0.,0.,-1.));
#3417=DIRECTION('center_axis',(0.,1.,0.));
#3418=DIRECTION('ref_axis',(0.,0.,-1.));
#3419=DIRECTION('center_axis',(0.,-1.,0.));
#3420=DIRECTION('ref_axis',(0.,0.,-1.));
#3421=DIRECTION('',(0.,1.,0.));
#3422=DIRECTION('center_axis',(0.,-1.,0.));
#3423=DIRECTION('ref_axis',(0.,0.,-1.));
#3424=DIRECTION('center_axis',(0.,1.,0.));
#3425=DIRECTION('ref_axis',(0.,0.,1.));
#3426=DIRECTION('center_axis',(0.,1.,0.));
#3427=DIRECTION('ref_axis',(0.,0.,1.));
#3428=DIRECTION('',(0.,1.,0.));
#3429=DIRECTION('center_axis',(0.,1.,0.));
#3430=DIRECTION('ref_axis',(0.,0.,1.));
#3431=DIRECTION('center_axis',(0.,1.,0.));
#3432=DIRECTION('ref_axis',(0.,0.,1.));
#3433=DIRECTION('center_axis',(0.,1.,0.));
#3434=DIRECTION('ref_axis',(0.,0.,1.));
#3435=DIRECTION('',(0.,1.,0.));
#3436=DIRECTION('center_axis',(0.,1.,0.));
#3437=DIRECTION('ref_axis',(0.,0.,1.));
#3438=DIRECTION('center_axis',(0.,1.,0.));
#3439=DIRECTION('ref_axis',(0.,0.,1.));
#3440=DIRECTION('center_axis',(0.,1.,0.));
#3441=DIRECTION('ref_axis',(0.,0.,1.));
#3442=DIRECTION('',(0.,1.,0.));
#3443=DIRECTION('center_axis',(0.,1.,0.));
#3444=DIRECTION('ref_axis',(0.,0.,1.));
#3445=DIRECTION('center_axis',(0.,1.,0.));
#3446=DIRECTION('ref_axis',(0.,0.,1.));
#3447=DIRECTION('center_axis',(0.,1.,0.));
#3448=DIRECTION('ref_axis',(0.,0.,1.));
#3449=DIRECTION('',(0.,1.,0.));
#3450=DIRECTION('center_axis',(0.,1.,0.));
#3451=DIRECTION('ref_axis',(0.,0.,1.));
#3452=DIRECTION('center_axis',(0.,1.,0.));
#3453=DIRECTION('ref_axis',(0.,0.,1.));
#3454=DIRECTION('center_axis',(0.,1.,0.));
#3455=DIRECTION('ref_axis',(0.,0.,1.));
#3456=DIRECTION('',(0.,1.,0.));
#3457=DIRECTION('center_axis',(0.,1.,0.));
#3458=DIRECTION('ref_axis',(0.,0.,1.));
#3459=DIRECTION('center_axis',(0.,1.,0.));
#3460=DIRECTION('ref_axis',(0.,0.,1.));
#3461=DIRECTION('',(1.,0.,0.));
#3462=DIRECTION('',(0.,0.,-1.));
#3463=DIRECTION('',(1.,0.,0.));
#3464=DIRECTION('',(0.,0.,-1.));
#3465=DIRECTION('center_axis',(0.,1.,0.));
#3466=DIRECTION('ref_axis',(0.,0.,1.));
#3467=DIRECTION('',(1.,0.,0.));
#3468=DIRECTION('',(0.,0.,-1.));
#3469=DIRECTION('',(1.,0.,0.));
#3470=DIRECTION('',(0.,0.,-1.));
#3471=DIRECTION('center_axis',(0.,1.,0.));
#3472=DIRECTION('ref_axis',(0.,0.,1.));
#3473=DIRECTION('',(0.,0.,-1.));
#3474=DIRECTION('',(1.,0.,0.));
#3475=DIRECTION('',(0.,0.,-1.));
#3476=DIRECTION('',(1.,0.,0.));
#3477=DIRECTION('center_axis',(1.,0.,0.));
#3478=DIRECTION('ref_axis',(0.,0.,-1.));
#3479=DIRECTION('',(0.,-1.,0.));
#3480=DIRECTION('',(0.,0.,-1.));
#3481=DIRECTION('',(0.,-1.,0.));
#3482=DIRECTION('',(0.,1.,0.));
#3483=DIRECTION('',(0.,0.,-1.));
#3484=DIRECTION('',(0.,1.,0.));
#3485=DIRECTION('',(0.,1.,0.));
#3486=DIRECTION('',(0.,0.,-1.));
#3487=DIRECTION('',(0.,1.,0.));
#3488=DIRECTION('center_axis',(0.,1.,0.));
#3489=DIRECTION('ref_axis',(0.,0.,1.));
#3490=DIRECTION('',(1.,0.,0.));
#3491=DIRECTION('',(0.,0.,-1.));
#3492=DIRECTION('',(1.,0.,0.));
#3493=DIRECTION('center_axis',(-1.,0.,0.));
#3494=DIRECTION('ref_axis',(0.,0.,1.));
#3495=DIRECTION('',(0.,1.,0.));
#3496=DIRECTION('',(0.,1.,0.));
#3497=DIRECTION('',(0.,0.,1.));
#3498=DIRECTION('',(0.,1.,0.));
#3499=DIRECTION('',(0.,1.,0.));
#3500=DIRECTION('',(0.,0.,1.));
#3501=DIRECTION('',(0.,1.,0.));
#3502=DIRECTION('',(0.,1.,0.));
#3503=DIRECTION('center_axis',(0.,0.,-1.));
#3504=DIRECTION('ref_axis',(-1.,0.,0.));
#3505=DIRECTION('center_axis',(0.,0.,-1.));
#3506=DIRECTION('ref_axis',(-1.,0.,0.));
#3507=DIRECTION('center_axis',(0.,0.,1.));
#3508=DIRECTION('ref_axis',(1.,0.,0.));
#3509=DIRECTION('',(1.,0.,0.));
#3510=DIRECTION('',(-1.,-2.19122965386544E-16,0.));
#3511=DIRECTION('center_axis',(0.,0.,1.));
#3512=DIRECTION('ref_axis',(1.,0.,0.));
#3513=DIRECTION('',(1.,1.46081976924363E-16,0.));
#3514=DIRECTION('center_axis',(0.,0.,1.));
#3515=DIRECTION('ref_axis',(1.,0.,0.));
#3516=DIRECTION('',(1.,0.,0.));
#3517=DIRECTION('center_axis',(0.,0.,1.));
#3518=DIRECTION('ref_axis',(1.,0.,0.));
#3519=DIRECTION('',(-1.,-2.19122965386544E-16,0.));
#3520=DIRECTION('',(1.,1.46081976924363E-16,0.));
#3521=DIRECTION('center_axis',(0.,1.,0.));
#3522=DIRECTION('ref_axis',(-1.,0.,0.));
#3523=DIRECTION('center_axis',(0.,0.,1.));
#3524=DIRECTION('ref_axis',(1.,0.,0.));
#3525=DIRECTION('',(1.,0.,0.));
#3526=DIRECTION('',(-1.,-2.19122965386544E-16,0.));
#3527=DIRECTION('center_axis',(0.,0.,1.));
#3528=DIRECTION('ref_axis',(1.,0.,0.));
#3529=DIRECTION('',(1.,1.46081976924363E-16,0.));
#3530=DIRECTION('center_axis',(0.,0.,1.));
#3531=DIRECTION('ref_axis',(1.,0.,0.));
#3532=DIRECTION('',(1.,0.,0.));
#3533=DIRECTION('center_axis',(0.,0.,1.));
#3534=DIRECTION('ref_axis',(1.,0.,0.));
#3535=DIRECTION('',(-1.,-2.19122965386544E-16,0.));
#3536=DIRECTION('',(1.,1.46081976924363E-16,0.));
#3537=DIRECTION('center_axis',(0.,1.,0.));
#3538=DIRECTION('ref_axis',(-1.,0.,0.));
#3539=DIRECTION('center_axis',(1.46081976924363E-16,-1.,0.));
#3540=DIRECTION('ref_axis',(1.,1.46081976924363E-16,0.));
#3541=DIRECTION('',(0.,0.,1.));
#3542=DIRECTION('center_axis',(-2.19122965386544E-16,1.,0.));
#3543=DIRECTION('ref_axis',(-1.,-2.19122965386544E-16,0.));
#3544=DIRECTION('',(0.,0.,1.));
#3545=DIRECTION('center_axis',(0.,0.,1.));
#3546=DIRECTION('ref_axis',(-1.,1.22464679914735E-16,0.));
#3547=DIRECTION('center_axis',(0.,0.,1.));
#3548=DIRECTION('ref_axis',(-1.,1.22464679914735E-16,0.));
#3549=DIRECTION('',(0.,0.,1.));
#3550=DIRECTION('',(0.,0.,1.));
#3551=DIRECTION('center_axis',(-2.19122965386544E-16,1.,0.));
#3552=DIRECTION('ref_axis',(-1.,-2.19122965386544E-16,0.));
#3553=DIRECTION('center_axis',(1.46081976924363E-16,-1.,0.));
#3554=DIRECTION('ref_axis',(1.,1.46081976924363E-16,0.));
#3555=DIRECTION('axis',(0.,0.,1.));
#3556=DIRECTION('refdir',(1.,0.,0.));
#3557=DIRECTION('center_axis',(0.,1.,0.));
#3558=DIRECTION('ref_axis',(0.,0.,1.));
#3559=DIRECTION('center_axis',(0.,1.,0.));
#3560=DIRECTION('ref_axis',(0.,0.,1.));
#3561=DIRECTION('',(0.,1.,0.));
#3562=DIRECTION('center_axis',(0.,1.,0.));
#3563=DIRECTION('ref_axis',(0.,0.,1.));
#3564=DIRECTION('center_axis',(0.,1.,0.));
#3565=DIRECTION('ref_axis',(0.,0.,1.));
#3566=DIRECTION('center_axis',(0.,1.,0.));
#3567=DIRECTION('ref_axis',(0.,0.,1.));
#3568=DIRECTION('',(0.,1.,0.));
#3569=DIRECTION('center_axis',(0.,1.,0.));
#3570=DIRECTION('ref_axis',(0.,0.,1.));
#3571=DIRECTION('center_axis',(0.,1.,0.));
#3572=DIRECTION('ref_axis',(0.,0.,1.));
#3573=DIRECTION('center_axis',(0.,1.,0.));
#3574=DIRECTION('ref_axis',(0.,0.,1.));
#3575=DIRECTION('',(0.,1.,0.));
#3576=DIRECTION('center_axis',(0.,1.,0.));
#3577=DIRECTION('ref_axis',(0.,0.,1.));
#3578=DIRECTION('center_axis',(0.,1.,0.));
#3579=DIRECTION('ref_axis',(0.,0.,1.));
#3580=DIRECTION('center_axis',(0.,1.,0.));
#3581=DIRECTION('ref_axis',(0.,0.,1.));
#3582=DIRECTION('',(0.,1.,0.));
#3583=DIRECTION('center_axis',(0.,1.,0.));
#3584=DIRECTION('ref_axis',(0.,0.,1.));
#3585=DIRECTION('center_axis',(0.,1.,0.));
#3586=DIRECTION('ref_axis',(0.,0.,1.));
#3587=DIRECTION('center_axis',(0.,1.,0.));
#3588=DIRECTION('ref_axis',(0.,0.,1.));
#3589=DIRECTION('',(0.,1.,0.));
#3590=DIRECTION('center_axis',(0.,1.,0.));
#3591=DIRECTION('ref_axis',(0.,0.,1.));
#3592=DIRECTION('center_axis',(0.,-1.,0.));
#3593=DIRECTION('ref_axis',(0.,0.,-1.));
#3594=DIRECTION('',(0.,0.,1.));
#3595=DIRECTION('',(1.,0.,0.));
#3596=DIRECTION('',(0.,0.,1.));
#3597=DIRECTION('',(1.,0.,0.));
#3598=DIRECTION('center_axis',(1.,0.,0.));
#3599=DIRECTION('ref_axis',(0.,0.,-1.));
#3600=DIRECTION('',(0.,1.,0.));
#3601=DIRECTION('',(0.,0.,1.));
#3602=DIRECTION('',(0.,1.,0.));
#3603=DIRECTION('center_axis',(0.,1.,0.));
#3604=DIRECTION('ref_axis',(0.,0.,1.));
#3605=DIRECTION('',(-1.,0.,0.));
#3606=DIRECTION('',(0.,0.,1.));
#3607=DIRECTION('',(-1.,0.,0.));
#3608=DIRECTION('center_axis',(-1.,0.,0.));
#3609=DIRECTION('ref_axis',(0.,0.,1.));
#3610=DIRECTION('',(0.,-1.,0.));
#3611=DIRECTION('',(0.,-1.,0.));
#3612=DIRECTION('center_axis',(0.,-1.,0.));
#3613=DIRECTION('ref_axis',(0.,0.,-1.));
#3614=DIRECTION('',(0.,0.,1.));
#3615=DIRECTION('',(1.,0.,0.));
#3616=DIRECTION('',(0.,0.,1.));
#3617=DIRECTION('',(1.,0.,0.));
#3618=DIRECTION('center_axis',(1.,0.,0.));
#3619=DIRECTION('ref_axis',(0.,0.,-1.));
#3620=DIRECTION('',(0.,1.,0.));
#3621=DIRECTION('',(0.,0.,1.));
#3622=DIRECTION('',(0.,1.,0.));
#3623=DIRECTION('center_axis',(0.,1.,0.));
#3624=DIRECTION('ref_axis',(0.,0.,1.));
#3625=DIRECTION('',(-1.,0.,0.));
#3626=DIRECTION('',(0.,0.,1.));
#3627=DIRECTION('',(-1.,0.,0.));
#3628=DIRECTION('center_axis',(-1.,0.,0.));
#3629=DIRECTION('ref_axis',(0.,0.,1.));
#3630=DIRECTION('',(0.,-1.,0.));
#3631=DIRECTION('',(0.,-1.,0.));
#3632=DIRECTION('center_axis',(0.,-1.,0.));
#3633=DIRECTION('ref_axis',(0.,0.,-1.));
#3634=DIRECTION('',(0.,0.,1.));
#3635=DIRECTION('',(1.,0.,0.));
#3636=DIRECTION('',(0.,0.,1.));
#3637=DIRECTION('',(1.,0.,0.));
#3638=DIRECTION('center_axis',(1.,0.,0.));
#3639=DIRECTION('ref_axis',(0.,0.,-1.));
#3640=DIRECTION('',(0.,1.,0.));
#3641=DIRECTION('',(0.,0.,1.));
#3642=DIRECTION('',(0.,1.,0.));
#3643=DIRECTION('center_axis',(0.,1.,0.));
#3644=DIRECTION('ref_axis',(0.,0.,1.));
#3645=DIRECTION('',(-1.,0.,0.));
#3646=DIRECTION('',(0.,0.,1.));
#3647=DIRECTION('',(-1.,0.,0.));
#3648=DIRECTION('center_axis',(-1.,0.,0.));
#3649=DIRECTION('ref_axis',(0.,0.,1.));
#3650=DIRECTION('',(0.,-1.,0.));
#3651=DIRECTION('',(0.,-1.,0.));
#3652=DIRECTION('center_axis',(0.,-1.,0.));
#3653=DIRECTION('ref_axis',(0.,0.,-1.));
#3654=DIRECTION('',(0.,0.,1.));
#3655=DIRECTION('',(1.,0.,0.));
#3656=DIRECTION('',(0.,0.,1.));
#3657=DIRECTION('',(1.,0.,0.));
#3658=DIRECTION('center_axis',(1.,0.,0.));
#3659=DIRECTION('ref_axis',(0.,0.,-1.));
#3660=DIRECTION('',(0.,1.,0.));
#3661=DIRECTION('',(0.,0.,1.));
#3662=DIRECTION('',(0.,1.,0.));
#3663=DIRECTION('center_axis',(0.,1.,0.));
#3664=DIRECTION('ref_axis',(0.,0.,1.));
#3665=DIRECTION('',(-1.,0.,0.));
#3666=DIRECTION('',(0.,0.,1.));
#3667=DIRECTION('',(-1.,0.,0.));
#3668=DIRECTION('center_axis',(-1.,0.,0.));
#3669=DIRECTION('ref_axis',(0.,0.,1.));
#3670=DIRECTION('',(0.,-1.,0.));
#3671=DIRECTION('',(0.,-1.,0.));
#3672=DIRECTION('center_axis',(1.,0.,0.));
#3673=DIRECTION('ref_axis',(0.,0.,-1.));
#3674=DIRECTION('',(0.,-1.,0.));
#3675=DIRECTION('',(0.,0.,1.));
#3676=DIRECTION('',(0.,1.,0.));
#3677=DIRECTION('',(0.,0.,1.));
#3678=DIRECTION('',(0.,-1.,0.));
#3679=DIRECTION('',(0.,0.,-1.));
#3680=DIRECTION('center_axis',(-1.,0.,0.));
#3681=DIRECTION('ref_axis',(0.,0.,1.));
#3682=DIRECTION('',(0.,1.,0.));
#3683=DIRECTION('',(0.,0.,-1.));
#3684=DIRECTION('',(0.,1.,0.));
#3685=DIRECTION('',(0.,0.,-1.));
#3686=DIRECTION('',(0.,1.,0.));
#3687=DIRECTION('',(0.,0.,-1.));
#3688=DIRECTION('center_axis',(0.,-1.,0.));
#3689=DIRECTION('ref_axis',(0.,0.,-1.));
#3690=DIRECTION('',(-1.,0.,0.));
#3691=DIRECTION('',(-1.,0.,0.));
#3692=DIRECTION('center_axis',(0.,0.,-1.));
#3693=DIRECTION('ref_axis',(-1.,0.,0.));
#3694=DIRECTION('',(-1.,0.,0.));
#3695=DIRECTION('',(1.,0.,0.));
#3696=DIRECTION('',(0.,-1.,0.));
#3697=DIRECTION('',(-1.,0.,0.));
#3698=DIRECTION('',(0.,1.,0.));
#3699=DIRECTION('',(1.,0.,0.));
#3700=DIRECTION('',(0.,-1.,0.));
#3701=DIRECTION('',(-1.,0.,0.));
#3702=DIRECTION('',(0.,1.,0.));
#3703=DIRECTION('center_axis',(0.,0.,-1.));
#3704=DIRECTION('ref_axis',(-1.,0.,0.));
#3705=DIRECTION('',(1.,0.,0.));
#3706=DIRECTION('',(0.,-1.,0.));
#3707=DIRECTION('',(1.,0.,0.));
#3708=DIRECTION('',(0.,1.,0.));
#3709=DIRECTION('',(-1.,0.,0.));
#3710=DIRECTION('',(0.,-1.,0.));
#3711=DIRECTION('',(1.,0.,0.));
#3712=DIRECTION('',(0.,1.,0.));
#3713=DIRECTION('',(-1.,0.,0.));
#3714=DIRECTION('center_axis',(0.,0.,1.));
#3715=DIRECTION('ref_axis',(1.,0.,0.));
#3716=DIRECTION('',(1.,0.,0.));
#3717=DIRECTION('',(1.,0.,0.));
#3718=DIRECTION('center_axis',(0.,1.,0.));
#3719=DIRECTION('ref_axis',(-1.,0.,0.));
#3720=DIRECTION('center_axis',(0.,1.,0.));
#3721=DIRECTION('ref_axis',(-1.,0.,0.));
#3722=DIRECTION('center_axis',(-1.,0.,0.));
#3723=DIRECTION('ref_axis',(0.,0.,1.));
#3724=DIRECTION('',(0.,0.,1.));
#3725=DIRECTION('',(0.,0.,1.));
#3726=DIRECTION('center_axis',(0.,1.,0.));
#3727=DIRECTION('ref_axis',(0.,0.,1.));
#3728=DIRECTION('',(0.,0.,1.));
#3729=DIRECTION('center_axis',(1.,0.,0.));
#3730=DIRECTION('ref_axis',(0.,0.,-1.));
#3731=DIRECTION('',(0.,0.,1.));
#3732=DIRECTION('center_axis',(0.,-1.,0.));
#3733=DIRECTION('ref_axis',(0.,0.,-1.));
#3734=DIRECTION('center_axis',(-1.,0.,0.));
#3735=DIRECTION('ref_axis',(0.,0.,1.));
#3736=DIRECTION('',(0.,0.,1.));
#3737=DIRECTION('',(0.,0.,1.));
#3738=DIRECTION('center_axis',(0.,1.,0.));
#3739=DIRECTION('ref_axis',(0.,0.,1.));
#3740=DIRECTION('',(0.,0.,1.));
#3741=DIRECTION('center_axis',(1.,0.,0.));
#3742=DIRECTION('ref_axis',(0.,0.,-1.));
#3743=DIRECTION('',(0.,0.,1.));
#3744=DIRECTION('center_axis',(0.,-1.,0.));
#3745=DIRECTION('ref_axis',(0.,0.,-1.));
#3746=DIRECTION('axis',(0.,0.,1.));
#3747=DIRECTION('refdir',(1.,0.,0.));
#3748=DIRECTION('center_axis',(0.,0.,-1.));
#3749=DIRECTION('ref_axis',(-1.,0.,0.));
#3750=DIRECTION('center_axis',(0.,0.,1.));
#3751=DIRECTION('ref_axis',(1.,0.,0.));
#3752=DIRECTION('center_axis',(0.,0.,1.));
#3753=DIRECTION('ref_axis',(1.,0.,0.));
#3754=DIRECTION('center_axis',(0.,0.,1.));
#3755=DIRECTION('ref_axis',(1.,0.,0.));
#3756=DIRECTION('',(0.,0.,1.));
#3757=DIRECTION('center_axis',(0.,0.,1.));
#3758=DIRECTION('ref_axis',(1.,0.,0.));
#3759=DIRECTION('center_axis',(0.,0.,1.));
#3760=DIRECTION('ref_axis',(1.,0.,0.));
#3761=DIRECTION('center_axis',(0.,0.,1.));
#3762=DIRECTION('ref_axis',(1.,0.,0.));
#3763=DIRECTION('center_axis',(0.,0.,1.));
#3764=DIRECTION('ref_axis',(1.,0.,0.));
#3765=DIRECTION('center_axis',(0.,0.,1.));
#3766=DIRECTION('ref_axis',(1.,0.,0.));
#3767=DIRECTION('center_axis',(0.,0.,1.));
#3768=DIRECTION('ref_axis',(1.,0.,0.));
#3769=DIRECTION('center_axis',(0.,0.,1.));
#3770=DIRECTION('ref_axis',(1.,0.,0.));
#3771=DIRECTION('center_axis',(0.,0.,1.));
#3772=DIRECTION('ref_axis',(1.,0.,0.));
#3773=DIRECTION('',(0.,-1.,0.));
#3774=DIRECTION('center_axis',(0.,0.,1.));
#3775=DIRECTION('ref_axis',(1.,0.,0.));
#3776=DIRECTION('',(1.,0.,0.));
#3777=DIRECTION('center_axis',(0.,0.,1.));
#3778=DIRECTION('ref_axis',(1.,0.,0.));
#3779=DIRECTION('',(0.,1.,0.));
#3780=DIRECTION('center_axis',(0.,0.,1.));
#3781=DIRECTION('ref_axis',(1.,0.,0.));
#3782=DIRECTION('',(-1.,0.,0.));
#3783=DIRECTION('center_axis',(0.,0.,1.));
#3784=DIRECTION('ref_axis',(1.,0.,0.));
#3785=DIRECTION('',(0.,-1.,0.));
#3786=DIRECTION('center_axis',(0.,0.,1.));
#3787=DIRECTION('ref_axis',(1.,0.,0.));
#3788=DIRECTION('',(1.,0.,0.));
#3789=DIRECTION('center_axis',(0.,0.,1.));
#3790=DIRECTION('ref_axis',(1.,0.,0.));
#3791=DIRECTION('',(0.,1.,0.));
#3792=DIRECTION('center_axis',(0.,0.,1.));
#3793=DIRECTION('ref_axis',(1.,0.,0.));
#3794=DIRECTION('',(-1.,0.,0.));
#3795=DIRECTION('center_axis',(0.,0.,1.));
#3796=DIRECTION('ref_axis',(1.,0.,0.));
#3797=DIRECTION('',(0.,1.,0.));
#3798=DIRECTION('',(1.,0.,0.));
#3799=DIRECTION('',(0.,-1.,0.));
#3800=DIRECTION('',(-1.,0.,0.));
#3801=DIRECTION('center_axis',(0.,1.,0.));
#3802=DIRECTION('ref_axis',(0.,0.,1.));
#3803=DIRECTION('',(0.,0.,-1.));
#3804=DIRECTION('',(0.,0.,-1.));
#3805=DIRECTION('center_axis',(1.,0.,0.));
#3806=DIRECTION('ref_axis',(0.,0.,-1.));
#3807=DIRECTION('',(0.,0.,-1.));
#3808=DIRECTION('center_axis',(0.,-1.,0.));
#3809=DIRECTION('ref_axis',(0.,0.,-1.));
#3810=DIRECTION('',(0.,0.,-1.));
#3811=DIRECTION('center_axis',(-1.,0.,0.));
#3812=DIRECTION('ref_axis',(0.,0.,1.));
#3813=DIRECTION('center_axis',(-1.,0.,0.));
#3814=DIRECTION('ref_axis',(0.,0.,1.));
#3815=DIRECTION('',(0.,0.,-1.));
#3816=DIRECTION('',(0.,1.,0.));
#3817=DIRECTION('',(0.,0.,-1.));
#3818=DIRECTION('center_axis',(0.,-1.,0.));
#3819=DIRECTION('ref_axis',(0.,0.,-1.));
#3820=DIRECTION('',(0.,0.,-1.));
#3821=DIRECTION('',(-1.,0.,0.));
#3822=DIRECTION('center_axis',(1.,0.,0.));
#3823=DIRECTION('ref_axis',(0.,0.,-1.));
#3824=DIRECTION('',(0.,0.,-1.));
#3825=DIRECTION('',(0.,-1.,0.));
#3826=DIRECTION('center_axis',(0.,1.,0.));
#3827=DIRECTION('ref_axis',(0.,0.,1.));
#3828=DIRECTION('',(1.,0.,0.));
#3829=DIRECTION('center_axis',(0.,0.,1.));
#3830=DIRECTION('ref_axis',(1.,0.,0.));
#3831=DIRECTION('axis',(0.,0.,1.));
#3832=DIRECTION('refdir',(1.,0.,0.));
#3833=DIRECTION('center_axis',(1.,0.,0.));
#3834=DIRECTION('ref_axis',(0.,0.,-1.));
#3835=DIRECTION('center_axis',(1.,0.,0.));
#3836=DIRECTION('ref_axis',(0.,0.,-1.));
#3837=DIRECTION('center_axis',(0.,-1.,-1.22464679914735E-16));
#3838=DIRECTION('ref_axis',(0.,-1.22464679914735E-16,1.));
#3839=DIRECTION('center_axis',(1.,0.,0.));
#3840=DIRECTION('ref_axis',(0.,0.,-1.));
#3841=DIRECTION('center_axis',(1.,0.,0.));
#3842=DIRECTION('ref_axis',(0.,0.,-1.));
#3843=DIRECTION('',(-1.,0.,0.));
#3844=DIRECTION('center_axis',(1.,0.,0.));
#3845=DIRECTION('ref_axis',(0.,0.,-1.));
#3846=DIRECTION('center_axis',(1.,0.,0.));
#3847=DIRECTION('ref_axis',(0.,0.,-1.));
#3848=DIRECTION('center_axis',(0.,-1.,-1.22464679914735E-16));
#3849=DIRECTION('ref_axis',(0.,-1.22464679914735E-16,1.));
#3850=DIRECTION('center_axis',(1.,0.,0.));
#3851=DIRECTION('ref_axis',(0.,0.,-1.));
#3852=DIRECTION('center_axis',(1.,0.,0.));
#3853=DIRECTION('ref_axis',(0.,0.,-1.));
#3854=DIRECTION('center_axis',(1.,0.,0.));
#3855=DIRECTION('ref_axis',(0.,0.,-1.));
#3856=DIRECTION('',(1.,0.,0.));
#3857=DIRECTION('center_axis',(-1.,0.,0.));
#3858=DIRECTION('ref_axis',(0.,0.,-1.));
#3859=DIRECTION('center_axis',(-1.,0.,0.));
#3860=DIRECTION('ref_axis',(0.,0.,-1.));
#3861=DIRECTION('center_axis',(1.,0.,0.));
#3862=DIRECTION('ref_axis',(0.,0.,-1.));
#3863=DIRECTION('center_axis',(1.,0.,0.));
#3864=DIRECTION('ref_axis',(0.,0.,1.));
#3865=DIRECTION('center_axis',(1.,0.,0.));
#3866=DIRECTION('ref_axis',(0.,0.,1.));
#3867=DIRECTION('',(1.,0.,0.));
#3868=DIRECTION('center_axis',(1.,0.,0.));
#3869=DIRECTION('ref_axis',(0.,0.,-1.));
#3870=DIRECTION('center_axis',(-1.,0.,0.));
#3871=DIRECTION('ref_axis',(0.,0.,1.));
#3872=DIRECTION('center_axis',(1.,0.,0.));
#3873=DIRECTION('ref_axis',(0.,0.,-1.));
#3874=DIRECTION('center_axis',(0.,-1.,1.22464679914735E-16));
#3875=DIRECTION('ref_axis',(0.,-1.22464679914735E-16,-1.));
#3876=DIRECTION('center_axis',(1.,0.,0.));
#3877=DIRECTION('ref_axis',(0.,0.,-1.));
#3878=DIRECTION('center_axis',(1.,0.,0.));
#3879=DIRECTION('ref_axis',(0.,0.,-1.));
#3880=DIRECTION('center_axis',(1.,0.,0.));
#3881=DIRECTION('ref_axis',(0.,0.,-1.));
#3882=DIRECTION('center_axis',(0.,-1.,-1.22464679914735E-16));
#3883=DIRECTION('ref_axis',(0.,-1.22464679914735E-16,1.));
#3884=DIRECTION('center_axis',(1.,0.,0.));
#3885=DIRECTION('ref_axis',(0.,0.,-1.));
#3886=DIRECTION('center_axis',(1.,0.,0.));
#3887=DIRECTION('ref_axis',(0.,0.,-1.));
#3888=DIRECTION('',(1.,0.,0.));
#3889=DIRECTION('center_axis',(1.,0.,0.));
#3890=DIRECTION('ref_axis',(0.,0.,-1.));
#3891=DIRECTION('center_axis',(1.,0.,0.));
#3892=DIRECTION('ref_axis',(0.,0.,-1.));
#3893=DIRECTION('center_axis',(0.,-1.,-1.22464679914735E-16));
#3894=DIRECTION('ref_axis',(0.,-1.22464679914735E-16,1.));
#3895=DIRECTION('center_axis',(1.,0.,0.));
#3896=DIRECTION('ref_axis',(0.,0.,-1.));
#3897=DIRECTION('center_axis',(1.,0.,0.));
#3898=DIRECTION('ref_axis',(0.,0.,-1.));
#3899=DIRECTION('',(-1.,0.,0.));
#3900=DIRECTION('center_axis',(1.,0.,0.));
#3901=DIRECTION('ref_axis',(0.,0.,-1.));
#3902=DIRECTION('center_axis',(1.,0.,0.));
#3903=DIRECTION('ref_axis',(0.,0.,-1.));
#3904=DIRECTION('center_axis',(1.,0.,0.));
#3905=DIRECTION('ref_axis',(0.,0.,-1.));
#3906=DIRECTION('',(-1.,0.,0.));
#3907=DIRECTION('center_axis',(-1.,0.,0.));
#3908=DIRECTION('ref_axis',(0.,0.,1.));
#3909=DIRECTION('center_axis',(-1.,0.,0.));
#3910=DIRECTION('ref_axis',(0.,0.,1.));
#3911=DIRECTION('center_axis',(-1.,0.,0.));
#3912=DIRECTION('ref_axis',(0.,0.,1.));
#3913=DIRECTION('center_axis',(0.,-1.,1.22464679914735E-16));
#3914=DIRECTION('ref_axis',(0.,-1.22464679914735E-16,-1.));
#3915=DIRECTION('center_axis',(1.,0.,0.));
#3916=DIRECTION('ref_axis',(0.,0.,-1.));
#3917=DIRECTION('center_axis',(-1.,0.,0.));
#3918=DIRECTION('ref_axis',(0.,0.,1.));
#3919=DIRECTION('center_axis',(1.,0.,0.));
#3920=DIRECTION('ref_axis',(0.,0.,-1.));
#3921=DIRECTION('center_axis',(-1.,0.,0.));
#3922=DIRECTION('ref_axis',(0.,0.,1.));
#3923=DIRECTION('axis',(0.,0.,1.));
#3924=DIRECTION('refdir',(1.,0.,0.));
#3925=DIRECTION('center_axis',(0.,0.,-1.));
#3926=DIRECTION('ref_axis',(-1.,0.,0.));
#3927=DIRECTION('center_axis',(0.,0.,1.));
#3928=DIRECTION('ref_axis',(1.,0.,0.));
#3929=DIRECTION('',(0.,0.,-1.));
#3930=DIRECTION('center_axis',(0.,0.,1.));
#3931=DIRECTION('ref_axis',(1.,0.,0.));
#3932=DIRECTION('center_axis',(0.,0.,1.));
#3933=DIRECTION('ref_axis',(1.,0.,0.));
#3934=DIRECTION('center_axis',(0.,0.,1.));
#3935=DIRECTION('ref_axis',(1.,0.,0.));
#3936=DIRECTION('',(0.,0.,1.));
#3937=DIRECTION('center_axis',(0.,0.,1.));
#3938=DIRECTION('ref_axis',(1.,0.,0.));
#3939=DIRECTION('center_axis',(0.,0.,-1.));
#3940=DIRECTION('ref_axis',(-1.,0.,0.));
#3941=DIRECTION('center_axis',(0.,0.,1.));
#3942=DIRECTION('ref_axis',(1.,0.,0.));
#3943=DIRECTION('',(0.,0.,1.));
#3944=DIRECTION('center_axis',(0.,0.,1.));
#3945=DIRECTION('ref_axis',(1.,0.,0.));
#3946=DIRECTION('center_axis',(0.,0.,-1.));
#3947=DIRECTION('ref_axis',(-1.,0.,0.));
#3948=DIRECTION('center_axis',(0.,0.,1.));
#3949=DIRECTION('ref_axis',(1.,0.,0.));
#3950=DIRECTION('',(0.,0.,-1.));
#3951=DIRECTION('center_axis',(0.,0.,-1.));
#3952=DIRECTION('ref_axis',(-1.,0.,0.));
#3953=DIRECTION('center_axis',(0.,0.,1.));
#3954=DIRECTION('ref_axis',(1.,0.,0.));
#3955=DIRECTION('center_axis',(0.,0.,1.));
#3956=DIRECTION('ref_axis',(1.,0.,0.));
#3957=DIRECTION('center_axis',(0.,0.,1.));
#3958=DIRECTION('ref_axis',(1.,0.,0.));
#3959=DIRECTION('center_axis',(0.,0.,-1.));
#3960=DIRECTION('ref_axis',(1.,0.,0.));
#3961=DIRECTION('axis',(0.,0.,1.));
#3962=DIRECTION('refdir',(1.,0.,0.));
#3963=DIRECTION('center_axis',(-1.,0.,0.));
#3964=DIRECTION('ref_axis',(0.,0.,1.));
#3965=DIRECTION('',(-0.500000000000005,-1.0605752387249E-16,-0.866025403784436));
#3966=DIRECTION('center_axis',(-1.,0.,0.));
#3967=DIRECTION('ref_axis',(0.,0.,1.));
#3968=DIRECTION('center_axis',(-1.,0.,0.));
#3969=DIRECTION('ref_axis',(0.,0.,1.));
#3970=DIRECTION('center_axis',(-1.,0.,0.));
#3971=DIRECTION('ref_axis',(0.,0.,1.));
#3972=DIRECTION('center_axis',(-1.,0.,0.));
#3973=DIRECTION('ref_axis',(0.,0.,1.));
#3974=DIRECTION('center_axis',(-1.,0.,0.));
#3975=DIRECTION('ref_axis',(0.,0.,1.));
#3976=DIRECTION('center_axis',(-1.,0.,0.));
#3977=DIRECTION('ref_axis',(0.,0.,1.));
#3978=DIRECTION('center_axis',(-1.,0.,0.));
#3979=DIRECTION('ref_axis',(0.,0.,1.));
#3980=DIRECTION('center_axis',(-1.,0.,0.));
#3981=DIRECTION('ref_axis',(0.,0.,1.));
#3982=DIRECTION('center_axis',(0.,-1.,1.22464679914735E-16));
#3983=DIRECTION('ref_axis',(0.,-1.22464679914735E-16,-1.));
#3984=DIRECTION('center_axis',(1.,0.,0.));
#3985=DIRECTION('ref_axis',(0.,0.,1.));
#3986=DIRECTION('center_axis',(1.,0.,0.));
#3987=DIRECTION('ref_axis',(0.,0.,-1.));
#3988=DIRECTION('center_axis',(1.,0.,0.));
#3989=DIRECTION('ref_axis',(0.,0.,-1.));
#3990=DIRECTION('center_axis',(1.,0.,0.));
#3991=DIRECTION('ref_axis',(0.,0.,-1.));
#3992=DIRECTION('center_axis',(0.,1.,1.22464679914735E-16));
#3993=DIRECTION('ref_axis',(0.,-1.22464679914735E-16,1.));
#3994=DIRECTION('center_axis',(-1.,0.,0.));
#3995=DIRECTION('ref_axis',(0.,0.,-1.));
#3996=DIRECTION('center_axis',(-1.,0.,0.));
#3997=DIRECTION('ref_axis',(0.,0.,1.));
#3998=DIRECTION('',(1.,0.,0.));
#3999=DIRECTION('center_axis',(-1.,0.,0.));
#4000=DIRECTION('ref_axis',(0.,0.,1.));
#4001=DIRECTION('center_axis',(-1.,0.,0.));
#4002=DIRECTION('ref_axis',(0.,0.,1.));
#4003=DIRECTION('',(1.,0.,0.));
#4004=DIRECTION('center_axis',(-1.,0.,0.));
#4005=DIRECTION('ref_axis',(0.,0.,1.));
#4006=DIRECTION('center_axis',(-1.,0.,0.));
#4007=DIRECTION('ref_axis',(0.,0.,1.));
#4008=DIRECTION('',(0.707106781186531,8.65956056235514E-17,0.707106781186564));
#4009=DIRECTION('center_axis',(-1.,0.,0.));
#4010=DIRECTION('ref_axis',(0.,0.,1.));
#4011=DIRECTION('center_axis',(-1.,0.,0.));
#4012=DIRECTION('ref_axis',(0.,0.,1.));
#4013=DIRECTION('',(0.,-0.499999999999999,0.866025403784439));
#4014=DIRECTION('',(0.,1.,-1.47141488612846E-15));
#4015=DIRECTION('',(0.,-0.500000000000001,-0.866025403784438));
#4016=DIRECTION('',(0.,0.499999999999999,-0.866025403784439));
#4017=DIRECTION('',(0.,-1.,1.2874880253624E-15));
#4018=DIRECTION('',(0.,-0.500000000000001,-0.866025403784438));
#4019=DIRECTION('center_axis',(1.,0.,0.));
#4020=DIRECTION('ref_axis',(0.,0.,-1.));
#4021=DIRECTION('center_axis',(1.,0.,0.));
#4022=DIRECTION('ref_axis',(0.,0.,-1.));
#4023=DIRECTION('center_axis',(0.,-0.866025403784439,-0.499999999999999));
#4024=DIRECTION('ref_axis',(0.,0.499999999999999,-0.866025403784439));
#4025=DIRECTION('',(-1.,0.,0.));
#4026=DIRECTION('',(0.,-0.499999999999999,0.866025403784439));
#4027=DIRECTION('',(0.,-0.499999999999999,0.866025403784439));
#4028=DIRECTION('',(-1.,0.,0.));
#4029=DIRECTION('center_axis',(0.,1.47141488612846E-15,1.));
#4030=DIRECTION('ref_axis',(0.,-1.,1.47141488612846E-15));
#4031=DIRECTION('',(0.,1.,-1.47141488612846E-15));
#4032=DIRECTION('',(0.,1.,-1.47141488612846E-15));
#4033=DIRECTION('',(-1.,0.,0.));
#4034=DIRECTION('center_axis',(0.,0.866025403784438,-0.500000000000001));
#4035=DIRECTION('ref_axis',(0.,0.500000000000001,0.866025403784438));
#4036=DIRECTION('',(0.,-0.500000000000001,-0.866025403784438));
#4037=DIRECTION('',(0.,-0.500000000000001,-0.866025403784438));
#4038=DIRECTION('',(-1.,0.,0.));
#4039=DIRECTION('center_axis',(0.,0.866025403784439,0.499999999999999));
#4040=DIRECTION('ref_axis',(0.,-0.499999999999999,0.866025403784439));
#4041=DIRECTION('',(0.,0.499999999999999,-0.866025403784439));
#4042=DIRECTION('',(0.,0.499999999999999,-0.866025403784439));
#4043=DIRECTION('',(-1.,0.,0.));
#4044=DIRECTION('center_axis',(0.,-1.2874880253624E-15,-1.));
#4045=DIRECTION('ref_axis',(0.,1.,-1.2874880253624E-15));
#4046=DIRECTION('',(0.,-1.,1.2874880253624E-15));
#4047=DIRECTION('',(0.,-1.,1.2874880253624E-15));
#4048=DIRECTION('',(-1.,0.,0.));
#4049=DIRECTION('center_axis',(0.,0.866025403784438,-0.500000000000001));
#4050=DIRECTION('ref_axis',(0.,0.500000000000001,0.866025403784438));
#4051=DIRECTION('',(0.,-0.500000000000001,-0.866025403784438));
#4052=DIRECTION('',(0.,-0.500000000000001,-0.866025403784438));
#4053=DIRECTION('center_axis',(1.,0.,0.));
#4054=DIRECTION('ref_axis',(0.,0.,-1.));
#4055=DIRECTION('center_axis',(1.,0.,0.));
#4056=DIRECTION('ref_axis',(0.,0.,-1.));
#4057=DIRECTION('center_axis',(1.,0.,0.));
#4058=DIRECTION('ref_axis',(0.,0.,-1.));
#4059=DIRECTION('center_axis',(1.,0.,0.));
#4060=DIRECTION('ref_axis',(0.,0.,-1.));
#4061=DIRECTION('center_axis',(1.,0.,0.));
#4062=DIRECTION('ref_axis',(0.,0.,-1.));
#4063=DIRECTION('center_axis',(1.,0.,0.));
#4064=DIRECTION('ref_axis',(0.,0.,-1.));
#4065=DIRECTION('axis',(0.,0.,1.));
#4066=DIRECTION('refdir',(1.,0.,0.));
#4067=DIRECTION('center_axis',(0.,0.,1.));
#4068=DIRECTION('ref_axis',(1.,0.,0.));
#4069=DIRECTION('center_axis',(0.,0.,1.));
#4070=DIRECTION('ref_axis',(-1.,0.,0.));
#4071=DIRECTION('',(0.,0.,1.));
#4072=DIRECTION('center_axis',(0.,0.,1.));
#4073=DIRECTION('ref_axis',(1.,0.,0.));
#4074=DIRECTION('center_axis',(0.,0.,1.));
#4075=DIRECTION('ref_axis',(1.,0.,0.));
#4076=DIRECTION('center_axis',(0.,0.,-1.));
#4077=DIRECTION('ref_axis',(-1.,0.,0.));
#4078=DIRECTION('center_axis',(0.,0.,1.));
#4079=DIRECTION('ref_axis',(-1.,0.,0.));
#4080=DIRECTION('',(0.81915204428899,-1.00317192905352E-16,-0.573576436351048));
#4081=DIRECTION('center_axis',(0.,0.,1.));
#4082=DIRECTION('ref_axis',(-1.,0.,0.));
#4083=DIRECTION('center_axis',(0.,0.,1.));
#4084=DIRECTION('ref_axis',(1.,0.,0.));
#4085=DIRECTION('center_axis',(0.,0.,-1.));
#4086=DIRECTION('ref_axis',(1.,0.,0.));
#4087=DIRECTION('',(-0.819152044288988,-1.00317192905352E-16,0.573576436351052));
#4088=DIRECTION('center_axis',(0.,0.,1.));
#4089=DIRECTION('ref_axis',(1.,0.,0.));
#4090=DIRECTION('center_axis',(0.,0.,-1.));
#4091=DIRECTION('ref_axis',(-1.,0.,0.));
#4092=DIRECTION('center_axis',(0.,0.,1.));
#4093=DIRECTION('ref_axis',(1.,0.,0.));
#4094=DIRECTION('',(-0.939692620785914,1.15079156022786E-16,0.342020143325654));
#4095=DIRECTION('center_axis',(0.,0.,1.));
#4096=DIRECTION('ref_axis',(1.,0.,0.));
#4097=DIRECTION('center_axis',(0.,0.,1.));
#4098=DIRECTION('ref_axis',(1.,0.,0.));
#4099=DIRECTION('center_axis',(1.22464679914735E-16,-1.,0.));
#4100=DIRECTION('ref_axis',(-1.,-1.22464679914735E-16,0.));
#4101=DIRECTION('center_axis',(0.,0.,1.));
#4102=DIRECTION('ref_axis',(1.,0.,0.));
#4103=DIRECTION('center_axis',(0.,0.,1.));
#4104=DIRECTION('ref_axis',(1.,0.,0.));
#4105=DIRECTION('',(0.,0.,1.));
#4106=DIRECTION('center_axis',(-0.500000000000002,0.866025403784438,0.));
#4107=DIRECTION('ref_axis',(-0.866025403784438,-0.500000000000002,0.));
#4108=DIRECTION('',(0.,0.,1.));
#4109=DIRECTION('',(0.,0.,1.));
#4110=DIRECTION('center_axis',(0.500000000000002,0.866025403784437,0.));
#4111=DIRECTION('ref_axis',(-0.866025403784437,0.500000000000002,0.));
#4112=DIRECTION('',(0.,0.,1.));
#4113=DIRECTION('center_axis',(-1.,0.,0.));
#4114=DIRECTION('ref_axis',(0.,0.,1.));
#4115=DIRECTION('',(0.,0.,1.));
#4116=DIRECTION('center_axis',(0.500000000000001,-0.866025403784438,0.));
#4117=DIRECTION('ref_axis',(0.866025403784438,0.500000000000001,0.));
#4118=DIRECTION('',(0.,0.,1.));
#4119=DIRECTION('center_axis',(-0.500000000000002,-0.866025403784438,0.));
#4120=DIRECTION('ref_axis',(0.866025403784437,-0.500000000000002,0.));
#4121=DIRECTION('',(0.,0.,1.));
#4122=DIRECTION('center_axis',(-1.,0.,0.));
#4123=DIRECTION('ref_axis',(0.,0.,1.));
#4124=DIRECTION('center_axis',(0.,0.,-1.));
#4125=DIRECTION('ref_axis',(-1.,0.,0.));
#4126=DIRECTION('center_axis',(0.,0.,-1.));
#4127=DIRECTION('ref_axis',(-1.,0.,0.));
#4128=DIRECTION('center_axis',(0.,0.,-1.));
#4129=DIRECTION('ref_axis',(-1.,0.,0.));
#4130=DIRECTION('center_axis',(0.,0.,-1.));
#4131=DIRECTION('ref_axis',(-1.,0.,0.));
#4132=DIRECTION('center_axis',(0.,0.,-1.));
#4133=DIRECTION('ref_axis',(-1.,0.,0.));
#4134=DIRECTION('center_axis',(0.,0.,1.));
#4135=DIRECTION('ref_axis',(1.,0.,0.));
#4136=DIRECTION('center_axis',(0.,0.,-1.));
#4137=DIRECTION('ref_axis',(-1.,0.,0.));
#4138=DIRECTION('center_axis',(0.,0.,-1.));
#4139=DIRECTION('ref_axis',(-1.,0.,0.));
#4140=DIRECTION('center_axis',(0.,0.,-1.));
#4141=DIRECTION('ref_axis',(-1.,0.,0.));
#4142=DIRECTION('center_axis',(0.,0.,-1.));
#4143=DIRECTION('ref_axis',(-1.,0.,0.));
#4144=DIRECTION('center_axis',(0.,0.,-1.));
#4145=DIRECTION('ref_axis',(-1.,0.,0.));
#4146=DIRECTION('center_axis',(0.,0.,-1.));
#4147=DIRECTION('ref_axis',(-1.,0.,0.));
#4148=DIRECTION('center_axis',(0.,0.,-1.));
#4149=DIRECTION('ref_axis',(-1.,0.,0.));
#4150=DIRECTION('center_axis',(0.,0.,-1.));
#4151=DIRECTION('ref_axis',(-1.,0.,0.));
#4152=DIRECTION('',(0.,0.,1.));
#4153=DIRECTION('',(1.,0.,0.));
#4154=DIRECTION('',(0.,0.,1.));
#4155=DIRECTION('',(1.,0.,0.));
#4156=DIRECTION('',(0.,0.,1.));
#4157=DIRECTION('',(1.,0.,0.));
#4158=DIRECTION('',(0.,0.,1.));
#4159=DIRECTION('',(1.,0.,0.));
#4160=DIRECTION('',(1.,0.,0.));
#4161=DIRECTION('',(0.,0.,-1.));
#4162=DIRECTION('',(0.,0.,1.));
#4163=DIRECTION('',(6.12323399573677E-17,-1.,0.));
#4164=DIRECTION('',(6.12323399573677E-17,-1.,0.));
#4165=DIRECTION('',(1.,6.12323399573677E-17,-6.12323399573676E-17));
#4166=DIRECTION('',(-1.,0.,0.));
#4167=DIRECTION('',(0.,0.,1.));
#4168=DIRECTION('',(0.,0.,1.));
#4169=DIRECTION('',(6.12323399573677E-17,-1.,0.));
#4170=DIRECTION('',(0.,0.,1.));
#4171=DIRECTION('',(6.12323399573677E-17,-1.,0.));
#4172=DIRECTION('',(0.,0.,1.));
#4173=DIRECTION('',(6.12323399573677E-17,-1.,0.));
#4174=DIRECTION('',(0.,0.,1.));
#4175=DIRECTION('',(6.12323399573677E-17,-1.,0.));
#4176=DIRECTION('',(6.12323399573677E-17,-1.,0.));
#4177=DIRECTION('',(1.,6.12323399573677E-17,-6.12323399573676E-17));
#4178=DIRECTION('',(6.12323399573677E-17,-1.,0.));
#4179=DIRECTION('',(1.,6.12323399573677E-17,-6.12323399573676E-17));
#4180=DIRECTION('',(6.12323399573677E-17,-1.,0.));
#4181=DIRECTION('',(1.,6.12323399573677E-17,-6.12323399573676E-17));
#4182=DIRECTION('',(6.12323399573677E-17,-1.,0.));
#4183=DIRECTION('',(1.,6.12323399573677E-17,-6.12323399573676E-17));
#4184=DIRECTION('',(0.,0.,-1.));
#4185=DIRECTION('',(-1.,0.,0.));
#4186=DIRECTION('',(-1.,0.,0.));
#4187=DIRECTION('',(0.,0.,1.));
#4188=DIRECTION('',(-1.,0.,0.));
#4189=DIRECTION('',(0.,0.,1.));
#4190=DIRECTION('',(-1.,0.,0.));
#4191=DIRECTION('',(0.,0.,1.));
#4192=DIRECTION('',(-1.,0.,0.));
#4193=DIRECTION('',(0.,0.,1.));
#4194=DIRECTION('',(-1.,0.,0.));
#4195=DIRECTION('',(0.,0.,1.));
#4196=DIRECTION('',(0.,0.,1.));
#4197=DIRECTION('',(1.,0.,0.));
#4198=DIRECTION('',(0.,0.,1.));
#4199=DIRECTION('',(1.,0.,0.));
#4200=DIRECTION('',(0.,0.,1.));
#4201=DIRECTION('',(1.,0.,0.));
#4202=DIRECTION('',(0.,0.,1.));
#4203=DIRECTION('',(1.,0.,0.));
#4204=DIRECTION('',(0.,0.,1.));
#4205=DIRECTION('',(1.,0.,0.));
#4206=DIRECTION('',(1.,0.,0.));
#4207=DIRECTION('',(0.,0.,-1.));
#4208=DIRECTION('',(1.,0.,0.));
#4209=DIRECTION('',(0.,0.,-1.));
#4210=DIRECTION('',(1.,0.,0.));
#4211=DIRECTION('',(0.,0.,-1.));
#4212=DIRECTION('',(1.,0.,0.));
#4213=DIRECTION('',(0.,0.,-1.));
#4214=DIRECTION('',(1.,0.,0.));
#4215=DIRECTION('',(0.,0.,-1.));
#4216=DIRECTION('',(0.,0.,1.));
#4217=DIRECTION('',(1.,0.,0.));
#4218=DIRECTION('',(0.,0.,1.));
#4219=DIRECTION('',(1.,0.,0.));
#4220=DIRECTION('',(0.,0.,1.));
#4221=DIRECTION('',(1.,0.,0.));
#4222=DIRECTION('',(0.,0.,1.));
#4223=DIRECTION('',(1.,0.,0.));
#4224=DIRECTION('',(0.,0.,1.));
#4225=DIRECTION('',(1.,0.,0.));
#4226=DIRECTION('',(6.12323399573677E-17,-1.,0.));
#4227=DIRECTION('',(-1.,-6.12323399573677E-17,-6.12323399573676E-17));
#4228=DIRECTION('',(6.12323399573677E-17,-1.,0.));
#4229=DIRECTION('',(-1.,-6.12323399573677E-17,-6.12323399573676E-17));
#4230=DIRECTION('',(0.,0.,1.));
#4231=DIRECTION('',(6.12323399573677E-17,-1.,0.));
#4232=DIRECTION('',(6.12323399573677E-17,-1.,0.));
#4233=DIRECTION('',(-1.,-6.12323399573677E-17,-6.12323399573676E-17));
#4234=DIRECTION('',(0.,0.,1.));
#4235=DIRECTION('',(6.12323399573677E-17,-1.,0.));
#4236=DIRECTION('',(0.,0.,1.));
#4237=DIRECTION('',(6.12323399573677E-17,-1.,0.));
#4238=DIRECTION('',(0.,0.,1.));
#4239=DIRECTION('',(6.12323399573677E-17,-1.,0.));
#4240=DIRECTION('',(0.,0.,1.));
#4241=DIRECTION('',(6.12323399573677E-17,-1.,0.));
#4242=DIRECTION('',(6.12323399573677E-17,-1.,0.));
#4243=DIRECTION('',(-1.,-6.12323399573677E-17,-6.12323399573676E-17));
#4244=DIRECTION('',(6.12323399573677E-17,-1.,0.));
#4245=DIRECTION('',(-1.,-6.12323399573677E-17,-6.12323399573676E-17));
#4246=CARTESIAN_POINT('',(0.,0.,0.));
#4247=CARTESIAN_POINT('',(0.,0.,0.));
#4248=CARTESIAN_POINT('Origin',(315.,-130.,-200.));
#4249=CARTESIAN_POINT('',(315.,-190.,-120.));
#4250=CARTESIAN_POINT('',(315.,-70.,-120.));
#4251=CARTESIAN_POINT('Origin',(315.,-130.,-120.));
#4252=CARTESIAN_POINT('',(315.,-190.,-100.));
#4253=CARTESIAN_POINT('',(315.,-190.,-200.));
#4254=CARTESIAN_POINT('',(315.,-70.,-100.));
#4255=CARTESIAN_POINT('Origin',(315.,-130.,-100.));
#4256=CARTESIAN_POINT('',(315.,-70.,-200.));
#4257=CARTESIAN_POINT('Origin',(315.,-130.,-200.));
#4258=CARTESIAN_POINT('',(315.,-190.,100.));
#4259=CARTESIAN_POINT('',(315.,-70.,100.));
#4260=CARTESIAN_POINT('Origin',(315.,-130.,100.));
#4261=CARTESIAN_POINT('',(315.,-190.,120.));
#4262=CARTESIAN_POINT('',(315.,-190.,-200.));
#4263=CARTESIAN_POINT('',(315.,-70.,120.));
#4264=CARTESIAN_POINT('Origin',(315.,-130.,120.));
#4265=CARTESIAN_POINT('',(315.,-70.,-200.));
#4266=CARTESIAN_POINT('Origin',(136.666666666667,-25.,-162.5));
#4267=CARTESIAN_POINT('',(136.666666666667,-30.,-159.85));
#4268=CARTESIAN_POINT('Origin',(136.666666666667,-30.,-162.5));
#4269=CARTESIAN_POINT('',(136.666666666667,-25.,-159.85));
#4270=CARTESIAN_POINT('',(136.666666666667,-25.,-159.85));
#4271=CARTESIAN_POINT('Origin',(136.666666666667,-25.,-162.5));
#4272=CARTESIAN_POINT('Origin',(220.,-25.,-162.5));
#4273=CARTESIAN_POINT('',(220.,-30.,-159.85));
#4274=CARTESIAN_POINT('Origin',(220.,-30.,-162.5));
#4275=CARTESIAN_POINT('',(220.,-25.,-159.85));
#4276=CARTESIAN_POINT('',(220.,-25.,-159.85));
#4277=CARTESIAN_POINT('Origin',(220.,-25.,-162.5));
#4278=CARTESIAN_POINT('Origin',(303.333333333333,-25.,-162.5));
#4279=CARTESIAN_POINT('',(303.333333333333,-30.,-159.85));
#4280=CARTESIAN_POINT('Origin',(303.333333333333,-30.,-162.5));
#4281=CARTESIAN_POINT('',(303.333333333333,-25.,-159.85));
#4282=CARTESIAN_POINT('',(303.333333333333,-25.,-159.85));
#4283=CARTESIAN_POINT('Origin',(303.333333333333,-25.,-162.5));
#4284=CARTESIAN_POINT('Origin',(386.666666666667,-25.,-162.5));
#4285=CARTESIAN_POINT('',(386.666666666667,-30.,-159.85));
#4286=CARTESIAN_POINT('Origin',(386.666666666667,-30.,-162.5));
#4287=CARTESIAN_POINT('',(386.666666666667,-25.,-159.85));
#4288=CARTESIAN_POINT('',(386.666666666667,-25.,-159.85));
#4289=CARTESIAN_POINT('Origin',(386.666666666667,-25.,-162.5));
#4290=CARTESIAN_POINT('Origin',(53.3333333333333,-25.,-162.5));
#4291=CARTESIAN_POINT('',(53.3333333333333,-30.,-159.85));
#4292=CARTESIAN_POINT('Origin',(53.3333333333333,-30.,-162.5));
#4293=CARTESIAN_POINT('',(53.3333333333333,-25.,-159.85));
#4294=CARTESIAN_POINT('',(53.3333333333333,-25.,-159.85));
#4295=CARTESIAN_POINT('Origin',(53.3333333333333,-25.,-162.5));
#4296=CARTESIAN_POINT('Origin',(53.3333333333333,-25.,162.5));
#4297=CARTESIAN_POINT('',(53.3333333333333,-30.,159.85));
#4298=CARTESIAN_POINT('Origin',(53.3333333333333,-30.,162.5));
#4299=CARTESIAN_POINT('',(53.3333333333333,-25.,159.85));
#4300=CARTESIAN_POINT('',(53.3333333333333,-25.,159.85));
#4301=CARTESIAN_POINT('Origin',(53.3333333333333,-25.,162.5));
#4302=CARTESIAN_POINT('Origin',(136.666666666667,-25.,162.5));
#4303=CARTESIAN_POINT('',(136.666666666667,-30.,159.85));
#4304=CARTESIAN_POINT('Origin',(136.666666666667,-30.,162.5));
#4305=CARTESIAN_POINT('',(136.666666666667,-25.,159.85));
#4306=CARTESIAN_POINT('',(136.666666666667,-25.,159.85));
#4307=CARTESIAN_POINT('Origin',(136.666666666667,-25.,162.5));
#4308=CARTESIAN_POINT('Origin',(220.,-25.,162.5));
#4309=CARTESIAN_POINT('',(220.,-30.,159.85));
#4310=CARTESIAN_POINT('Origin',(220.,-30.,162.5));
#4311=CARTESIAN_POINT('',(220.,-25.,159.85));
#4312=CARTESIAN_POINT('',(220.,-25.,159.85));
#4313=CARTESIAN_POINT('Origin',(220.,-25.,162.5));
#4314=CARTESIAN_POINT('Origin',(303.333333333333,-25.,162.5));
#4315=CARTESIAN_POINT('',(303.333333333333,-30.,159.85));
#4316=CARTESIAN_POINT('Origin',(303.333333333333,-30.,162.5));
#4317=CARTESIAN_POINT('',(303.333333333333,-25.,159.85));
#4318=CARTESIAN_POINT('',(303.333333333333,-25.,159.85));
#4319=CARTESIAN_POINT('Origin',(303.333333333333,-25.,162.5));
#4320=CARTESIAN_POINT('Origin',(386.666666666667,-25.,162.5));
#4321=CARTESIAN_POINT('',(386.666666666667,-30.,159.85));
#4322=CARTESIAN_POINT('Origin',(386.666666666667,-30.,162.5));
#4323=CARTESIAN_POINT('',(386.666666666667,-25.,159.85));
#4324=CARTESIAN_POINT('',(386.666666666667,-25.,159.85));
#4325=CARTESIAN_POINT('Origin',(386.666666666667,-25.,162.5));
#4326=CARTESIAN_POINT('Origin',(-30.,-30.,200.));
#4327=CARTESIAN_POINT('',(-30.,-30.,100.));
#4328=CARTESIAN_POINT('',(470.,-30.,100.));
#4329=CARTESIAN_POINT('',(-30.,-30.,100.));
#4330=CARTESIAN_POINT('',(-30.,-30.,-100.));
#4331=CARTESIAN_POINT('',(-30.,-30.,200.));
#4332=CARTESIAN_POINT('',(470.,-30.,-100.));
#4333=CARTESIAN_POINT('',(-30.,-30.,-100.));
#4334=CARTESIAN_POINT('',(470.,-30.,200.));
#4335=CARTESIAN_POINT('Origin',(-30.,-30.,200.));
#4336=CARTESIAN_POINT('',(-30.,-30.,-120.));
#4337=CARTESIAN_POINT('',(470.,-30.,-120.));
#4338=CARTESIAN_POINT('',(-30.,-30.,-120.));
#4339=CARTESIAN_POINT('',(-30.,-30.,-200.));
#4340=CARTESIAN_POINT('',(-30.,-30.,200.));
#4341=CARTESIAN_POINT('',(470.,-30.,-200.));
#4342=CARTESIAN_POINT('',(-30.,-30.,-200.));
#4343=CARTESIAN_POINT('',(470.,-30.,200.));
#4344=CARTESIAN_POINT('Origin',(-30.,-30.,200.));
#4345=CARTESIAN_POINT('',(-30.,-30.,200.));
#4346=CARTESIAN_POINT('',(-30.,-30.,120.));
#4347=CARTESIAN_POINT('',(-30.,-30.,200.));
#4348=CARTESIAN_POINT('',(470.,-30.,120.));
#4349=CARTESIAN_POINT('',(-30.,-30.,120.));
#4350=CARTESIAN_POINT('',(470.,-30.,200.));
#4351=CARTESIAN_POINT('',(470.,-30.,200.));
#4352=CARTESIAN_POINT('',(-30.,-30.,200.));
#4353=CARTESIAN_POINT('Origin',(470.,-25.,200.));
#4354=CARTESIAN_POINT('',(470.,-25.,-200.));
#4355=CARTESIAN_POINT('',(470.,-25.,-200.));
#4356=CARTESIAN_POINT('',(470.,-25.,200.));
#4357=CARTESIAN_POINT('',(470.,-25.,200.));
#4358=CARTESIAN_POINT('',(470.,-25.,200.));
#4359=CARTESIAN_POINT('',(470.,-230.,120.));
#4360=CARTESIAN_POINT('',(470.,-230.,120.));
#4361=CARTESIAN_POINT('',(470.,-230.,100.));
#4362=CARTESIAN_POINT('',(470.,-230.,120.));
#4363=CARTESIAN_POINT('',(470.,-230.,100.));
#4364=CARTESIAN_POINT('',(470.,-230.,-100.));
#4365=CARTESIAN_POINT('',(470.,-230.,-100.));
#4366=CARTESIAN_POINT('',(470.,-230.,-120.));
#4367=CARTESIAN_POINT('',(470.,-230.,-100.));
#4368=CARTESIAN_POINT('',(470.,-230.,-120.));
#4369=CARTESIAN_POINT('Origin',(-30.,-25.,200.));
#4370=CARTESIAN_POINT('',(-30.,-25.,-200.));
#4371=CARTESIAN_POINT('',(-30.,-25.,-200.));
#4372=CARTESIAN_POINT('',(-30.,-25.,200.));
#4373=CARTESIAN_POINT('',(-30.,-25.,200.));
#4374=CARTESIAN_POINT('',(-30.,-25.,200.));
#4375=CARTESIAN_POINT('Origin',(-30.,-30.,200.));
#4376=CARTESIAN_POINT('',(-30.,-30.,-200.));
#4377=CARTESIAN_POINT('',(-30.,-230.,-120.));
#4378=CARTESIAN_POINT('',(-30.,-230.,-120.));
#4379=CARTESIAN_POINT('',(-30.,-230.,-100.));
#4380=CARTESIAN_POINT('',(-30.,-230.,-120.));
#4381=CARTESIAN_POINT('',(-30.,-230.,-100.));
#4382=CARTESIAN_POINT('',(-30.,-230.,100.));
#4383=CARTESIAN_POINT('',(-30.,-230.,100.));
#4384=CARTESIAN_POINT('',(-30.,-230.,120.));
#4385=CARTESIAN_POINT('',(-30.,-230.,100.));
#4386=CARTESIAN_POINT('',(-30.,-230.,120.));
#4387=CARTESIAN_POINT('',(-30.,-30.,200.));
#4388=CARTESIAN_POINT('Origin',(0.,0.,200.));
#4389=CARTESIAN_POINT('Origin',(0.,0.,-200.));
#4390=CARTESIAN_POINT('Origin',(-30.,-230.,-120.));
#4391=CARTESIAN_POINT('',(-30.,-230.,-120.));
#4392=CARTESIAN_POINT('',(125.,-70.0000000000001,-120.));
#4393=CARTESIAN_POINT('',(-30.0000000000001,-70.0000000000001,-120.));
#4394=CARTESIAN_POINT('',(125.,-190.,-120.));
#4395=CARTESIAN_POINT('Origin',(125.,-130.,-120.));
#4396=CARTESIAN_POINT('',(-30.,-190.,-120.));
#4397=CARTESIAN_POINT('Origin',(-30.,-230.,-100.));
#4398=CARTESIAN_POINT('',(-30.,-230.,-100.));
#4399=CARTESIAN_POINT('',(125.,-70.0000000000001,-100.));
#4400=CARTESIAN_POINT('',(125.,-190.,-100.));
#4401=CARTESIAN_POINT('Origin',(125.,-130.,-100.));
#4402=CARTESIAN_POINT('',(-30.0000000000001,-70.0000000000001,-100.));
#4403=CARTESIAN_POINT('',(-30.,-190.,-100.));
#4404=CARTESIAN_POINT('Origin',(0.,-230.,0.));
#4405=CARTESIAN_POINT('Origin',(-30.,-230.,100.));
#4406=CARTESIAN_POINT('',(-30.,-230.,100.));
#4407=CARTESIAN_POINT('',(125.,-70.0000000000001,100.));
#4408=CARTESIAN_POINT('',(-30.0000000000001,-70.0000000000001,100.));
#4409=CARTESIAN_POINT('',(125.,-190.,100.));
#4410=CARTESIAN_POINT('Origin',(125.,-130.,100.));
#4411=CARTESIAN_POINT('',(-30.,-190.,100.));
#4412=CARTESIAN_POINT('Origin',(-30.,-230.,120.));
#4413=CARTESIAN_POINT('',(-30.,-230.,120.));
#4414=CARTESIAN_POINT('',(125.,-70.0000000000001,120.));
#4415=CARTESIAN_POINT('',(125.,-190.,120.));
#4416=CARTESIAN_POINT('Origin',(125.,-130.,120.));
#4417=CARTESIAN_POINT('',(-30.0000000000001,-70.0000000000001,120.));
#4418=CARTESIAN_POINT('',(-30.,-190.,120.));
#4419=CARTESIAN_POINT('Origin',(0.,-230.,0.));
#4420=CARTESIAN_POINT('Origin',(125.,-190.,-200.));
#4421=CARTESIAN_POINT('',(125.,-190.,-200.));
#4422=CARTESIAN_POINT('Origin',(125.,-70.0000000000001,-200.));
#4423=CARTESIAN_POINT('',(125.,-70.0000000000001,-200.));
#4424=CARTESIAN_POINT('Origin',(125.,-130.,-200.));
#4425=CARTESIAN_POINT('Origin',(125.,-130.,-200.));
#4426=CARTESIAN_POINT('',(125.,-70.0000000000001,-200.));
#4427=CARTESIAN_POINT('',(125.,-190.,-200.));
#4428=CARTESIAN_POINT('Origin',(125.,-70.0000000000001,-200.));
#4429=CARTESIAN_POINT('Origin',(125.,-190.,-200.));
#4430=CARTESIAN_POINT('',(0.,0.,0.));
#4431=CARTESIAN_POINT('Origin',(53.3333333333333,-20.,162.5));
#4432=CARTESIAN_POINT('',(53.3333333333333,-25.,159.85));
#4433=CARTESIAN_POINT('Origin',(53.3333333333333,-25.,162.5));
#4434=CARTESIAN_POINT('',(53.3333333333333,-20.,159.85));
#4435=CARTESIAN_POINT('',(53.3333333333333,-20.,159.85));
#4436=CARTESIAN_POINT('Origin',(53.3333333333333,-20.,162.5));
#4437=CARTESIAN_POINT('Origin',(136.666666666667,-20.,162.5));
#4438=CARTESIAN_POINT('',(136.666666666667,-25.,159.85));
#4439=CARTESIAN_POINT('Origin',(136.666666666667,-25.,162.5));
#4440=CARTESIAN_POINT('',(136.666666666667,-20.,159.85));
#4441=CARTESIAN_POINT('',(136.666666666667,-20.,159.85));
#4442=CARTESIAN_POINT('Origin',(136.666666666667,-20.,162.5));
#4443=CARTESIAN_POINT('Origin',(220.,-20.,162.5));
#4444=CARTESIAN_POINT('',(220.,-25.,159.85));
#4445=CARTESIAN_POINT('Origin',(220.,-25.,162.5));
#4446=CARTESIAN_POINT('',(220.,-20.,159.85));
#4447=CARTESIAN_POINT('',(220.,-20.,159.85));
#4448=CARTESIAN_POINT('Origin',(220.,-20.,162.5));
#4449=CARTESIAN_POINT('Origin',(303.333333333333,-20.,162.5));
#4450=CARTESIAN_POINT('',(303.333333333333,-25.,159.85));
#4451=CARTESIAN_POINT('Origin',(303.333333333333,-25.,162.5));
#4452=CARTESIAN_POINT('',(303.333333333333,-20.,159.85));
#4453=CARTESIAN_POINT('',(303.333333333333,-20.,159.85));
#4454=CARTESIAN_POINT('Origin',(303.333333333333,-20.,162.5));
#4455=CARTESIAN_POINT('Origin',(386.666666666667,-20.,162.5));
#4456=CARTESIAN_POINT('',(386.666666666667,-25.,159.85));
#4457=CARTESIAN_POINT('Origin',(386.666666666667,-25.,162.5));
#4458=CARTESIAN_POINT('',(386.666666666667,-20.,159.85));
#4459=CARTESIAN_POINT('',(386.666666666667,-20.,159.85));
#4460=CARTESIAN_POINT('Origin',(386.666666666667,-20.,162.5));
#4461=CARTESIAN_POINT('Origin',(435.,-8.66025403784439,139.999));
#4462=CARTESIAN_POINT('',(435.,-8.66025403784439,140.));
#4463=CARTESIAN_POINT('',(435.,-8.66025403784439,145.));
#4464=CARTESIAN_POINT('',(435.,-8.66025403784439,139.999));
#4465=CARTESIAN_POINT('',(445.,-8.66025403784439,145.));
#4466=CARTESIAN_POINT('',(435.,-8.66025403784439,145.));
#4467=CARTESIAN_POINT('',(445.,-8.66025403784439,140.));
#4468=CARTESIAN_POINT('',(445.,-8.66025403784439,139.999));
#4469=CARTESIAN_POINT('',(435.,-8.66025403784439,140.));
#4470=CARTESIAN_POINT('Origin',(445.,8.66025403784439,139.999));
#4471=CARTESIAN_POINT('',(445.,8.66025403784439,145.));
#4472=CARTESIAN_POINT('',(445.,8.66025403784439,145.));
#4473=CARTESIAN_POINT('',(445.,8.66025403784439,140.));
#4474=CARTESIAN_POINT('',(445.,8.66025403784439,139.999));
#4475=CARTESIAN_POINT('',(445.,8.66025403784439,140.));
#4476=CARTESIAN_POINT('Origin',(435.,8.66025403784439,139.999));
#4477=CARTESIAN_POINT('',(435.,8.66025403784439,145.));
#4478=CARTESIAN_POINT('',(435.,8.66025403784439,145.));
#4479=CARTESIAN_POINT('',(435.,8.66025403784439,140.));
#4480=CARTESIAN_POINT('',(435.,8.66025403784439,139.999));
#4481=CARTESIAN_POINT('',(435.,8.66025403784439,140.));
#4482=CARTESIAN_POINT('Origin',(435.,8.66025403784439,139.999));
#4483=CARTESIAN_POINT('',(435.,8.66025403784439,145.));
#4484=CARTESIAN_POINT('',(435.,8.66025403784439,140.));
#4485=CARTESIAN_POINT('Origin',(347.,-8.66025403784439,139.999));
#4486=CARTESIAN_POINT('',(347.,-8.66025403784439,140.));
#4487=CARTESIAN_POINT('',(347.,-8.66025403784439,145.));
#4488=CARTESIAN_POINT('',(347.,-8.66025403784439,139.999));
#4489=CARTESIAN_POINT('',(357.,-8.66025403784439,145.));
#4490=CARTESIAN_POINT('',(347.,-8.66025403784439,145.));
#4491=CARTESIAN_POINT('',(357.,-8.66025403784439,140.));
#4492=CARTESIAN_POINT('',(357.,-8.66025403784439,139.999));
#4493=CARTESIAN_POINT('',(347.,-8.66025403784439,140.));
#4494=CARTESIAN_POINT('Origin',(357.,8.66025403784439,139.999));
#4495=CARTESIAN_POINT('',(357.,8.66025403784439,145.));
#4496=CARTESIAN_POINT('',(357.,8.66025403784439,145.));
#4497=CARTESIAN_POINT('',(357.,8.66025403784439,140.));
#4498=CARTESIAN_POINT('',(357.,8.66025403784439,139.999));
#4499=CARTESIAN_POINT('',(357.,8.66025403784439,140.));
#4500=CARTESIAN_POINT('Origin',(347.,8.66025403784439,139.999));
#4501=CARTESIAN_POINT('',(347.,8.66025403784439,145.));
#4502=CARTESIAN_POINT('',(347.,8.66025403784439,145.));
#4503=CARTESIAN_POINT('',(347.,8.66025403784439,140.));
#4504=CARTESIAN_POINT('',(347.,8.66025403784439,139.999));
#4505=CARTESIAN_POINT('',(347.,8.66025403784439,140.));
#4506=CARTESIAN_POINT('Origin',(347.,8.66025403784439,139.999));
#4507=CARTESIAN_POINT('',(347.,8.66025403784439,145.));
#4508=CARTESIAN_POINT('',(347.,8.66025403784439,140.));
#4509=CARTESIAN_POINT('Origin',(259.,-8.66025403784439,139.999));
#4510=CARTESIAN_POINT('',(259.,-8.66025403784439,140.));
#4511=CARTESIAN_POINT('',(259.,-8.66025403784439,145.));
#4512=CARTESIAN_POINT('',(259.,-8.66025403784439,139.999));
#4513=CARTESIAN_POINT('',(269.,-8.66025403784439,145.));
#4514=CARTESIAN_POINT('',(259.,-8.66025403784439,145.));
#4515=CARTESIAN_POINT('',(269.,-8.66025403784439,140.));
#4516=CARTESIAN_POINT('',(269.,-8.66025403784439,139.999));
#4517=CARTESIAN_POINT('',(259.,-8.66025403784439,140.));
#4518=CARTESIAN_POINT('Origin',(269.,8.66025403784439,139.999));
#4519=CARTESIAN_POINT('',(269.,8.66025403784439,145.));
#4520=CARTESIAN_POINT('',(269.,8.66025403784439,145.));
#4521=CARTESIAN_POINT('',(269.,8.66025403784439,140.));
#4522=CARTESIAN_POINT('',(269.,8.66025403784439,139.999));
#4523=CARTESIAN_POINT('',(269.,8.66025403784439,140.));
#4524=CARTESIAN_POINT('Origin',(259.,8.66025403784439,139.999));
#4525=CARTESIAN_POINT('',(259.,8.66025403784439,145.));
#4526=CARTESIAN_POINT('',(259.,8.66025403784439,145.));
#4527=CARTESIAN_POINT('',(259.,8.66025403784439,140.));
#4528=CARTESIAN_POINT('',(259.,8.66025403784439,139.999));
#4529=CARTESIAN_POINT('',(259.,8.66025403784439,140.));
#4530=CARTESIAN_POINT('Origin',(259.,8.66025403784439,139.999));
#4531=CARTESIAN_POINT('',(259.,8.66025403784439,145.));
#4532=CARTESIAN_POINT('',(259.,8.66025403784439,140.));
#4533=CARTESIAN_POINT('Origin',(171.,-8.66025403784439,139.999));
#4534=CARTESIAN_POINT('',(171.,-8.66025403784439,140.));
#4535=CARTESIAN_POINT('',(171.,-8.66025403784439,145.));
#4536=CARTESIAN_POINT('',(171.,-8.66025403784439,139.999));
#4537=CARTESIAN_POINT('',(181.,-8.66025403784439,145.));
#4538=CARTESIAN_POINT('',(171.,-8.66025403784439,145.));
#4539=CARTESIAN_POINT('',(181.,-8.66025403784439,140.));
#4540=CARTESIAN_POINT('',(181.,-8.66025403784439,139.999));
#4541=CARTESIAN_POINT('',(171.,-8.66025403784439,140.));
#4542=CARTESIAN_POINT('Origin',(181.,8.66025403784439,139.999));
#4543=CARTESIAN_POINT('',(181.,8.66025403784439,145.));
#4544=CARTESIAN_POINT('',(181.,8.66025403784439,145.));
#4545=CARTESIAN_POINT('',(181.,8.66025403784439,140.));
#4546=CARTESIAN_POINT('',(181.,8.66025403784439,139.999));
#4547=CARTESIAN_POINT('',(181.,8.66025403784439,140.));
#4548=CARTESIAN_POINT('Origin',(171.,8.66025403784439,139.999));
#4549=CARTESIAN_POINT('',(171.,8.66025403784439,145.));
#4550=CARTESIAN_POINT('',(171.,8.66025403784439,145.));
#4551=CARTESIAN_POINT('',(171.,8.66025403784439,140.));
#4552=CARTESIAN_POINT('',(171.,8.66025403784439,139.999));
#4553=CARTESIAN_POINT('',(171.,8.66025403784439,140.));
#4554=CARTESIAN_POINT('Origin',(171.,8.66025403784439,139.999));
#4555=CARTESIAN_POINT('',(171.,8.66025403784439,145.));
#4556=CARTESIAN_POINT('',(171.,8.66025403784439,140.));
#4557=CARTESIAN_POINT('Origin',(-30.,0.,145.));
#4558=CARTESIAN_POINT('',(-30.,20.,140.));
#4559=CARTESIAN_POINT('',(-30.,-25.,140.));
#4560=CARTESIAN_POINT('',(-30.,0.,140.));
#4561=CARTESIAN_POINT('',(-30.,-25.,180.));
#4562=CARTESIAN_POINT('',(-30.,-25.,140.));
#4563=CARTESIAN_POINT('',(-30.,-20.,180.));
#4564=CARTESIAN_POINT('',(-30.,-25.,180.));
#4565=CARTESIAN_POINT('',(-30.,-20.,145.));
#4566=CARTESIAN_POINT('',(-30.,-20.,140.));
#4567=CARTESIAN_POINT('',(-30.,20.,145.));
#4568=CARTESIAN_POINT('',(-30.,0.,145.));
#4569=CARTESIAN_POINT('',(-30.,20.,145.));
#4570=CARTESIAN_POINT('Origin',(470.,0.,145.));
#4571=CARTESIAN_POINT('',(470.,-25.,140.));
#4572=CARTESIAN_POINT('',(470.,20.,140.));
#4573=CARTESIAN_POINT('',(470.,0.,140.));
#4574=CARTESIAN_POINT('',(470.,20.,145.));
#4575=CARTESIAN_POINT('',(470.,20.,145.));
#4576=CARTESIAN_POINT('',(470.,-20.,145.));
#4577=CARTESIAN_POINT('',(470.,0.,145.));
#4578=CARTESIAN_POINT('',(470.,-20.,180.));
#4579=CARTESIAN_POINT('',(470.,-20.,180.));
#4580=CARTESIAN_POINT('',(470.,-25.,180.));
#4581=CARTESIAN_POINT('',(470.,-25.,180.));
#4582=CARTESIAN_POINT('',(470.,-25.,180.));
#4583=CARTESIAN_POINT('Origin',(0.,20.,145.));
#4584=CARTESIAN_POINT('',(0.,20.,140.));
#4585=CARTESIAN_POINT('',(0.,20.,145.));
#4586=CARTESIAN_POINT('Origin',(0.,0.,145.));
#4587=CARTESIAN_POINT('',(0.,-20.,145.));
#4588=CARTESIAN_POINT('',(83.,-8.66025403784439,145.));
#4589=CARTESIAN_POINT('',(93.,-8.66025403784439,145.));
#4590=CARTESIAN_POINT('',(83.,-8.66025403784439,145.));
#4591=CARTESIAN_POINT('',(83.,8.66025403784439,145.));
#4592=CARTESIAN_POINT('',(83.,8.66025403784439,145.));
#4593=CARTESIAN_POINT('',(93.,8.66025403784439,145.));
#4594=CARTESIAN_POINT('',(83.,8.66025403784439,145.));
#4595=CARTESIAN_POINT('',(93.,8.66025403784439,145.));
#4596=CARTESIAN_POINT('',(-5.,-8.66025403784439,145.));
#4597=CARTESIAN_POINT('',(5.,-8.66025403784439,145.));
#4598=CARTESIAN_POINT('',(-5.,-8.66025403784439,145.));
#4599=CARTESIAN_POINT('',(-5.,8.66025403784439,145.));
#4600=CARTESIAN_POINT('',(-5.,8.66025403784439,145.));
#4601=CARTESIAN_POINT('',(5.,8.66025403784439,145.));
#4602=CARTESIAN_POINT('',(-5.,8.66025403784439,145.));
#4603=CARTESIAN_POINT('',(5.,8.66025403784439,145.));
#4604=CARTESIAN_POINT('Origin',(0.,0.,140.));
#4605=CARTESIAN_POINT('',(-30.,-25.,140.));
#4606=CARTESIAN_POINT('',(83.,8.66025403784439,140.));
#4607=CARTESIAN_POINT('',(83.,-8.66025403784439,140.));
#4608=CARTESIAN_POINT('',(83.,8.66025403784439,140.));
#4609=CARTESIAN_POINT('',(93.,-8.66025403784439,140.));
#4610=CARTESIAN_POINT('',(83.,-8.66025403784439,140.));
#4611=CARTESIAN_POINT('',(93.,8.66025403784439,140.));
#4612=CARTESIAN_POINT('',(93.,8.66025403784439,140.));
#4613=CARTESIAN_POINT('',(83.,8.66025403784439,140.));
#4614=CARTESIAN_POINT('',(-5.,8.66025403784439,140.));
#4615=CARTESIAN_POINT('',(-5.,-8.66025403784439,140.));
#4616=CARTESIAN_POINT('',(-5.,8.66025403784439,140.));
#4617=CARTESIAN_POINT('',(5.,-8.66025403784439,140.));
#4618=CARTESIAN_POINT('',(-5.,-8.66025403784439,140.));
#4619=CARTESIAN_POINT('',(5.,8.66025403784439,140.));
#4620=CARTESIAN_POINT('',(5.,8.66025403784439,140.));
#4621=CARTESIAN_POINT('',(-5.,8.66025403784439,140.));
#4622=CARTESIAN_POINT('Origin',(-30.,-25.,180.));
#4623=CARTESIAN_POINT('',(-30.,-20.,180.));
#4624=CARTESIAN_POINT('',(-30.,-25.,180.));
#4625=CARTESIAN_POINT('Origin',(0.,-25.,0.));
#4626=CARTESIAN_POINT('Origin',(0.,-20.,0.));
#4627=CARTESIAN_POINT('Origin',(-5.,8.66025403784439,139.999));
#4628=CARTESIAN_POINT('',(-5.,8.66025403784439,139.999));
#4629=CARTESIAN_POINT('',(-5.,-8.66025403784439,139.999));
#4630=CARTESIAN_POINT('Origin',(-5.,8.66025403784439,139.999));
#4631=CARTESIAN_POINT('',(5.,8.66025403784439,139.999));
#4632=CARTESIAN_POINT('Origin',(5.,8.66025403784439,139.999));
#4633=CARTESIAN_POINT('',(5.,-8.66025403784439,139.999));
#4634=CARTESIAN_POINT('Origin',(-5.,-8.66025403784439,139.999));
#4635=CARTESIAN_POINT('Origin',(83.,8.66025403784439,139.999));
#4636=CARTESIAN_POINT('',(83.,8.66025403784439,139.999));
#4637=CARTESIAN_POINT('',(83.,-8.66025403784439,139.999));
#4638=CARTESIAN_POINT('Origin',(83.,8.66025403784439,139.999));
#4639=CARTESIAN_POINT('',(93.,8.66025403784439,139.999));
#4640=CARTESIAN_POINT('Origin',(93.,8.66025403784439,139.999));
#4641=CARTESIAN_POINT('',(93.,-8.66025403784439,139.999));
#4642=CARTESIAN_POINT('Origin',(83.,-8.66025403784439,139.999));
#4643=CARTESIAN_POINT('',(0.,0.,0.));
#4644=CARTESIAN_POINT('Origin',(0.,0.,140.));
#4645=CARTESIAN_POINT('',(-5.,8.66025403784439,-140.));
#4646=CARTESIAN_POINT('',(-5.,-8.66025403784439,-140.));
#4647=CARTESIAN_POINT('Origin',(0.,0.,-140.));
#4648=CARTESIAN_POINT('',(5.,-8.66025403784439,-140.));
#4649=CARTESIAN_POINT('Origin',(0.,0.,-140.));
#4650=CARTESIAN_POINT('',(10.,-1.22464679914735E-15,-140.));
#4651=CARTESIAN_POINT('Origin',(0.,0.,-140.));
#4652=CARTESIAN_POINT('',(10.,-1.22464679914735E-15,140.));
#4653=CARTESIAN_POINT('',(10.,-1.22464679914735E-15,140.));
#4654=CARTESIAN_POINT('',(5.,-8.66025403784439,140.));
#4655=CARTESIAN_POINT('Origin',(0.,0.,140.));
#4656=CARTESIAN_POINT('',(-5.,-8.66025403784439,140.));
#4657=CARTESIAN_POINT('Origin',(0.,0.,140.));
#4658=CARTESIAN_POINT('',(-5.,8.66025403784439,140.));
#4659=CARTESIAN_POINT('Origin',(0.,0.,140.));
#4660=CARTESIAN_POINT('',(5.,8.66025403784439,140.));
#4661=CARTESIAN_POINT('Origin',(0.,0.,140.));
#4662=CARTESIAN_POINT('Origin',(0.,0.,140.));
#4663=CARTESIAN_POINT('',(4.99999999999999,8.66025403784439,-140.));
#4664=CARTESIAN_POINT('Origin',(0.,0.,-140.));
#4665=CARTESIAN_POINT('Origin',(0.,0.,-140.));
#4666=CARTESIAN_POINT('Origin',(0.,0.,140.));
#4667=CARTESIAN_POINT('',(5.,0.,140.));
#4668=CARTESIAN_POINT('Origin',(0.,0.,140.));
#4669=CARTESIAN_POINT('',(0.,8.66025403784439,140.));
#4670=CARTESIAN_POINT('Origin',(0.,0.,140.));
#4671=CARTESIAN_POINT('',(-5.,0.,140.));
#4672=CARTESIAN_POINT('Origin',(0.,0.,140.));
#4673=CARTESIAN_POINT('',(0.,-8.66025403784439,140.));
#4674=CARTESIAN_POINT('Origin',(0.,0.,-140.));
#4675=CARTESIAN_POINT('',(5.,0.,-140.));
#4676=CARTESIAN_POINT('Origin',(0.,0.,-140.));
#4677=CARTESIAN_POINT('',(0.,8.66025403784439,-140.));
#4678=CARTESIAN_POINT('Origin',(0.,0.,-140.));
#4679=CARTESIAN_POINT('',(-5.,0.,-140.));
#4680=CARTESIAN_POINT('Origin',(0.,0.,-140.));
#4681=CARTESIAN_POINT('',(0.,-8.66025403784439,-140.));
#4682=CARTESIAN_POINT('Origin',(0.,0.,-150.));
#4683=CARTESIAN_POINT('',(5.,-8.66025403784439,-150.));
#4684=CARTESIAN_POINT('',(5.,8.66025403784439,-150.));
#4685=CARTESIAN_POINT('',(5.,8.66025403784439,-150.));
#4686=CARTESIAN_POINT('',(-5.,-8.66025403784439,-150.));
#4687=CARTESIAN_POINT('',(-5.,-8.66025403784439,-150.));
#4688=CARTESIAN_POINT('',(-5.,8.66025403784439,-150.));
#4689=CARTESIAN_POINT('',(-5.,8.66025403784439,-150.));
#4690=CARTESIAN_POINT('',(-5.,8.66025403784439,-150.));
#4691=CARTESIAN_POINT('Origin',(-5.,-8.66025403784439,150.));
#4692=CARTESIAN_POINT('',(5.,-8.66025403784439,150.));
#4693=CARTESIAN_POINT('',(-5.,-8.66025403784439,150.));
#4694=CARTESIAN_POINT('Origin',(-5.,8.66025403784439,150.));
#4695=CARTESIAN_POINT('',(-5.,8.66025403784439,150.));
#4696=CARTESIAN_POINT('Origin',(-5.,8.66025403784439,150.));
#4697=CARTESIAN_POINT('',(5.,8.66025403784439,150.));
#4698=CARTESIAN_POINT('Origin',(5.,8.66025403784439,150.));
#4699=CARTESIAN_POINT('Origin',(5.,8.66025403784439,150.));
#4700=CARTESIAN_POINT('',(5.,8.66025403784439,150.));
#4701=CARTESIAN_POINT('',(5.,8.66025403784439,150.));
#4702=CARTESIAN_POINT('',(5.,-8.66025403784439,150.));
#4703=CARTESIAN_POINT('',(5.,8.66025403784439,150.));
#4704=CARTESIAN_POINT('',(5.,-8.66025403784439,150.));
#4705=CARTESIAN_POINT('Origin',(-5.,8.66025403784439,150.));
#4706=CARTESIAN_POINT('',(-5.,8.66025403784439,150.));
#4707=CARTESIAN_POINT('',(-5.,8.66025403784439,150.));
#4708=CARTESIAN_POINT('',(-5.,8.66025403784439,150.));
#4709=CARTESIAN_POINT('Origin',(-5.,8.66025403784439,150.));
#4710=CARTESIAN_POINT('',(-5.,-8.66025403784439,150.));
#4711=CARTESIAN_POINT('',(-5.,-8.66025403784439,150.));
#4712=CARTESIAN_POINT('',(-5.,8.66025403784439,150.));
#4713=CARTESIAN_POINT('Origin',(-5.,-8.66025403784439,150.));
#4714=CARTESIAN_POINT('',(-5.,-8.66025403784439,150.));
#4715=CARTESIAN_POINT('Origin',(0.,0.,150.));
#4716=CARTESIAN_POINT('',(0.,0.,0.));
#4717=CARTESIAN_POINT('Origin',(1.8,0.,0.));
#4718=CARTESIAN_POINT('',(2.,-1.62878024286598E-15,13.3));
#4719=CARTESIAN_POINT('Origin',(2.,0.,0.));
#4720=CARTESIAN_POINT('',(1.8,-1.65327317884893E-15,13.5));
#4721=CARTESIAN_POINT('Origin',(1.8,-1.62878024286598E-15,13.3));
#4722=CARTESIAN_POINT('Origin',(1.8,0.,0.));
#4723=CARTESIAN_POINT('Origin',(-20.6375,0.,0.));
#4724=CARTESIAN_POINT('',(-1.80000000000001,-1.65327317884893E-15,13.5));
#4725=CARTESIAN_POINT('',(-20.6375,-1.65327317884893E-15,13.5));
#4726=CARTESIAN_POINT('Origin',(-1.8,0.,0.));
#4727=CARTESIAN_POINT('Origin',(-1.8,0.,0.));
#4728=CARTESIAN_POINT('',(-2.,-1.62878024286598E-15,13.3));
#4729=CARTESIAN_POINT('Origin',(-1.8,-1.62878024286598E-15,13.3));
#4730=CARTESIAN_POINT('Origin',(-2.,0.,0.));
#4731=CARTESIAN_POINT('Origin',(-20.6375,0.,0.));
#4732=CARTESIAN_POINT('',(-2.,-1.56448628591074E-15,12.775));
#4733=CARTESIAN_POINT('Origin',(-2.,0.,0.));
#4734=CARTESIAN_POINT('',(-0.227760839478619,-1.56448628591074E-15,12.775));
#4735=CARTESIAN_POINT('',(-20.6375,-1.56448628591074E-15,12.775));
#4736=CARTESIAN_POINT('',(-0.227760839478618,1.56448628591074E-15,-12.775));
#4737=CARTESIAN_POINT('Origin',(-0.227760839478618,0.,0.));
#4738=CARTESIAN_POINT('Origin',(-0.227760839478618,0.,0.));
#4739=CARTESIAN_POINT('Origin',(-20.6375,0.,0.));
#4740=CARTESIAN_POINT('',(0.782623792124928,1.52468526493845E-15,-12.45));
#4741=CARTESIAN_POINT('',(0.782623792124926,-1.52468526493846E-15,12.45));
#4742=CARTESIAN_POINT('Origin',(0.782623792124928,0.,0.));
#4743=CARTESIAN_POINT('Origin',(0.782623792124928,0.,0.));
#4744=CARTESIAN_POINT('',(2.,-1.52468526493846E-15,12.45));
#4745=CARTESIAN_POINT('',(-20.6375,-1.52468526493846E-15,12.45));
#4746=CARTESIAN_POINT('Origin',(2.,0.,0.));
#4747=CARTESIAN_POINT('Origin',(0.,0.,0.));
#4748=CARTESIAN_POINT('',(-0.782623792124928,1.35323471305783E-15,11.05));
#4749=CARTESIAN_POINT('',(-0.782623792124928,-1.35323471305783E-15,-11.05));
#4750=CARTESIAN_POINT('Origin',(-0.782623792124928,0.,0.));
#4751=CARTESIAN_POINT('Origin',(0.,-1.43895998899814E-15,-11.75));
#4752=CARTESIAN_POINT('Origin',(-0.782623792124928,0.,0.));
#4753=CARTESIAN_POINT('Origin',(-1.8,0.,0.));
#4754=CARTESIAN_POINT('',(-2.,-1.2491397351303E-15,10.2));
#4755=CARTESIAN_POINT('Origin',(-2.,0.,0.));
#4756=CARTESIAN_POINT('',(-1.8,-1.22464679914735E-15,10.));
#4757=CARTESIAN_POINT('Origin',(-1.8,-1.2491397351303E-15,10.2));
#4758=CARTESIAN_POINT('Origin',(-1.8,0.,0.));
#4759=CARTESIAN_POINT('Origin',(-20.6375,0.,0.));
#4760=CARTESIAN_POINT('',(1.8,-1.22464679914735E-15,10.));
#4761=CARTESIAN_POINT('',(-20.6375,-1.22464679914735E-15,10.));
#4762=CARTESIAN_POINT('Origin',(1.8,0.,0.));
#4763=CARTESIAN_POINT('Origin',(1.8,0.,0.));
#4764=CARTESIAN_POINT('',(2.,-1.2491397351303E-15,10.2));
#4765=CARTESIAN_POINT('Origin',(1.8,-1.2491397351303E-15,10.2));
#4766=CARTESIAN_POINT('Origin',(2.,0.,0.));
#4767=CARTESIAN_POINT('Origin',(-20.6375,0.,0.));
#4768=CARTESIAN_POINT('',(-2.,-1.35323471305783E-15,11.05));
#4769=CARTESIAN_POINT('',(-20.6375,-1.35323471305783E-15,11.05));
#4770=CARTESIAN_POINT('Origin',(-2.,0.,0.));
#4771=CARTESIAN_POINT('Origin',(-20.6375,0.,0.));
#4772=CARTESIAN_POINT('',(2.,-1.31343369208554E-15,10.725));
#4773=CARTESIAN_POINT('Origin',(2.,0.,0.));
#4774=CARTESIAN_POINT('',(0.227760839478619,-1.31343369208554E-15,10.725));
#4775=CARTESIAN_POINT('',(-20.6375,-1.31343369208554E-15,10.725));
#4776=CARTESIAN_POINT('',(0.227760839478618,1.419059478512E-15,-10.725));
#4777=CARTESIAN_POINT('Origin',(0.227760839478618,0.,0.));
#4778=CARTESIAN_POINT('Origin',(0.227760839478618,0.,0.));
#4779=CARTESIAN_POINT('Origin',(0.,0.,0.));
#4780=CARTESIAN_POINT('Origin',(0.,-1.43895998899814E-15,-11.75));
#4781=CARTESIAN_POINT('Origin',(2.,10.2,0.));
#4782=CARTESIAN_POINT('Origin',(-2.,11.05,0.));
#4783=CARTESIAN_POINT('Origin',(2.,13.3,0.));
#4784=CARTESIAN_POINT('Origin',(-2.,12.775,0.));
#4785=CARTESIAN_POINT('',(0.,0.,0.));
#4786=CARTESIAN_POINT('Origin',(0.,0.,-121.));
#4787=CARTESIAN_POINT('',(13.5,-1.65327317884893E-15,-121.));
#4788=CARTESIAN_POINT('Origin',(0.,0.,-121.));
#4789=CARTESIAN_POINT('',(13.5,-1.65327317884893E-15,-125.));
#4790=CARTESIAN_POINT('',(13.5,-1.65327317884893E-15,-121.));
#4791=CARTESIAN_POINT('Origin',(0.,0.,-125.));
#4792=CARTESIAN_POINT('Origin',(0.,0.,121.));
#4793=CARTESIAN_POINT('',(-13.5,-1.65327317884893E-15,121.));
#4794=CARTESIAN_POINT('Origin',(0.,0.,121.));
#4795=CARTESIAN_POINT('',(-13.5,-1.65327317884893E-15,125.));
#4796=CARTESIAN_POINT('',(-13.5,-1.65327317884893E-15,121.));
#4797=CARTESIAN_POINT('Origin',(0.,0.,125.));
#4798=CARTESIAN_POINT('Origin',(0.,0.,125.));
#4799=CARTESIAN_POINT('',(22.5,-2.75545529808155E-15,-125.));
#4800=CARTESIAN_POINT('Origin',(0.,0.,-125.));
#4801=CARTESIAN_POINT('',(22.5,-2.75545529808155E-15,125.));
#4802=CARTESIAN_POINT('',(22.5,-2.75545529808155E-15,125.));
#4803=CARTESIAN_POINT('Origin',(0.,0.,125.));
#4804=CARTESIAN_POINT('Origin',(0.,0.,125.));
#4805=CARTESIAN_POINT('',(10.5,-1.28587913910472E-15,121.));
#4806=CARTESIAN_POINT('Origin',(0.,0.,121.));
#4807=CARTESIAN_POINT('',(10.5,-1.28587913910472E-15,-121.));
#4808=CARTESIAN_POINT('',(10.5,-1.28587913910472E-15,125.));
#4809=CARTESIAN_POINT('Origin',(0.,0.,-121.));
#4810=CARTESIAN_POINT('Origin',(0.,0.,125.));
#4811=CARTESIAN_POINT('Origin',(0.,0.,-125.));
#4812=CARTESIAN_POINT('Origin',(0.,0.,121.));
#4813=CARTESIAN_POINT('Origin',(0.,0.,-121.));
#4814=CARTESIAN_POINT('',(0.,0.,0.));
#4815=CARTESIAN_POINT('Origin',(2.5,0.,0.));
#4816=CARTESIAN_POINT('',(3.67894924968523,0.,0.));
#4817=CARTESIAN_POINT('',(2.5,-2.62905054779003E-15,-2.042));
#4818=CARTESIAN_POINT('',(2.5,-2.50072876385889E-16,-2.042));
#4819=CARTESIAN_POINT('',(2.5,-1.76842387452782,-1.021));
#4820=CARTESIAN_POINT('Origin',(2.5,0.,0.));
#4821=CARTESIAN_POINT('',(2.5,-1.76842387452782,1.021));
#4822=CARTESIAN_POINT('Origin',(2.5,0.,0.));
#4823=CARTESIAN_POINT('',(2.5,3.00462919747432E-15,2.042));
#4824=CARTESIAN_POINT('Origin',(2.5,0.,0.));
#4825=CARTESIAN_POINT('',(2.5,1.76842387452782,1.021));
#4826=CARTESIAN_POINT('Origin',(2.5,0.,0.));
#4827=CARTESIAN_POINT('',(2.5,1.76842387452782,-1.021));
#4828=CARTESIAN_POINT('Origin',(2.5,0.,0.));
#4829=CARTESIAN_POINT('Origin',(2.5,0.,0.));
#4830=CARTESIAN_POINT('Origin',(0.25,0.,0.));
#4831=CARTESIAN_POINT('',(0.,-4.89858719658941E-16,-4.));
#4832=CARTESIAN_POINT('Origin',(0.,0.,0.));
#4833=CARTESIAN_POINT('',(0.25,-5.20474889637625E-16,-4.25));
#4834=CARTESIAN_POINT('Origin',(0.25,-4.89858719658941E-16,-4.));
#4835=CARTESIAN_POINT('Origin',(0.25,0.,0.));
#4836=CARTESIAN_POINT('Origin',(5.2,0.,0.));
#4837=CARTESIAN_POINT('',(5.2,3.06161699786838E-16,-2.5));
#4838=CARTESIAN_POINT('',(5.2,-3.06161699786838E-16,2.5));
#4839=CARTESIAN_POINT('Origin',(5.2,0.,0.));
#4840=CARTESIAN_POINT('Origin',(5.2,0.,0.));
#4841=CARTESIAN_POINT('',(5.,-3.30654635769785E-16,2.7));
#4842=CARTESIAN_POINT('Origin',(5.2,-3.30654635769785E-16,2.7));
#4843=CARTESIAN_POINT('Origin',(5.,0.,0.));
#4844=CARTESIAN_POINT('Origin',(-31.75,0.,0.));
#4845=CARTESIAN_POINT('',(5.,-5.20474889637625E-16,-4.25));
#4846=CARTESIAN_POINT('',(-31.75,-5.20474889637625E-16,-4.25));
#4847=CARTESIAN_POINT('Origin',(5.,0.,0.));
#4848=CARTESIAN_POINT('Origin',(-31.75,0.,0.));
#4849=CARTESIAN_POINT('',(24.555,-3.06161699786838E-16,-2.5));
#4850=CARTESIAN_POINT('',(-31.75,-3.06161699786838E-16,-2.5));
#4851=CARTESIAN_POINT('Origin',(24.555,0.,0.));
#4852=CARTESIAN_POINT('Origin',(25.,0.,0.));
#4853=CARTESIAN_POINT('',(25.,-2.51664917224781E-16,-2.055));
#4854=CARTESIAN_POINT('',(25.,-2.51664917224781E-16,-2.055));
#4855=CARTESIAN_POINT('Origin',(25.,0.,0.));
#4856=CARTESIAN_POINT('Origin',(0.,0.,0.));
#4857=CARTESIAN_POINT('',(0.,2.35789849937043,-1.95156391047391E-15));
#4858=CARTESIAN_POINT('',(0.,1.17894924968522,2.042));
#4859=CARTESIAN_POINT('',(0.,2.35789849937043,-1.95156391047391E-15));
#4860=CARTESIAN_POINT('',(0.,-1.17894924968521,2.042));
#4861=CARTESIAN_POINT('',(0.,-1.17894924968521,2.042));
#4862=CARTESIAN_POINT('',(0.,-2.35789849937043,3.25260651745651E-15));
#4863=CARTESIAN_POINT('',(0.,-1.17894924968521,2.042));
#4864=CARTESIAN_POINT('',(0.,-1.17894924968522,-2.042));
#4865=CARTESIAN_POINT('',(0.,-2.35789849937043,3.25260651745651E-15));
#4866=CARTESIAN_POINT('',(0.,1.17894924968521,-2.042));
#4867=CARTESIAN_POINT('',(0.,1.17894924968521,-2.042));
#4868=CARTESIAN_POINT('',(0.,2.35789849937043,-1.95156391047391E-15));
#4869=CARTESIAN_POINT('Origin',(25.,2.055,0.));
#4870=CARTESIAN_POINT('Origin',(5.,4.25,0.));
#4871=CARTESIAN_POINT('Origin',(2.5,2.35789849937043,-1.95156391047391E-15));
#4872=CARTESIAN_POINT('',(2.5,2.35789849937043,-1.95156391047391E-15));
#4873=CARTESIAN_POINT('',(2.5,2.35789849937043,-1.95156391047391E-15));
#4874=CARTESIAN_POINT('',(2.5,2.35789849937043,-1.95156391047391E-15));
#4875=CARTESIAN_POINT('',(2.5,1.17894924968522,2.042));
#4876=CARTESIAN_POINT('',(2.5,2.35789849937043,-1.95156391047391E-15));
#4877=CARTESIAN_POINT('',(2.5,1.17894924968522,2.042));
#4878=CARTESIAN_POINT('Origin',(2.5,-1.17894924968521,2.042));
#4879=CARTESIAN_POINT('',(2.5,-1.17894924968521,2.042));
#4880=CARTESIAN_POINT('',(2.5,-1.17894924968521,2.042));
#4881=CARTESIAN_POINT('',(2.5,-1.17894924968521,2.042));
#4882=CARTESIAN_POINT('',(2.5,-1.17894924968521,2.042));
#4883=CARTESIAN_POINT('Origin',(2.5,-1.17894924968521,2.042));
#4884=CARTESIAN_POINT('',(2.5,-1.17894924968521,2.042));
#4885=CARTESIAN_POINT('',(2.5,-2.35789849937043,3.25260651745651E-15));
#4886=CARTESIAN_POINT('',(2.5,-1.17894924968521,2.042));
#4887=CARTESIAN_POINT('',(2.5,-2.35789849937043,3.25260651745651E-15));
#4888=CARTESIAN_POINT('Origin',(2.5,-2.35789849937043,3.25260651745651E-15));
#4889=CARTESIAN_POINT('',(2.5,-2.35789849937043,3.25260651745651E-15));
#4890=CARTESIAN_POINT('',(2.5,-1.17894924968522,-2.042));
#4891=CARTESIAN_POINT('',(2.5,-2.35789849937043,3.25260651745651E-15));
#4892=CARTESIAN_POINT('',(2.5,-1.17894924968522,-2.042));
#4893=CARTESIAN_POINT('Origin',(2.5,1.17894924968521,-2.042));
#4894=CARTESIAN_POINT('',(2.5,1.17894924968521,-2.042));
#4895=CARTESIAN_POINT('',(2.5,1.17894924968521,-2.042));
#4896=CARTESIAN_POINT('',(2.5,1.17894924968521,-2.042));
#4897=CARTESIAN_POINT('',(2.5,1.17894924968521,-2.042));
#4898=CARTESIAN_POINT('Origin',(2.5,2.35789849937043,-1.95156391047391E-15));
#4899=CARTESIAN_POINT('',(2.5,2.35789849937043,-1.95156391047391E-15));
#4900=CARTESIAN_POINT('',(2.5,2.35789849937043,-1.95156391047391E-15));
#4901=CARTESIAN_POINT('Origin',(2.5,2.35789849937043,-1.95156391047391E-15));
#4902=CARTESIAN_POINT('Origin',(2.5,2.35789849937043,-1.95156391047391E-15));
#4903=CARTESIAN_POINT('Origin',(2.5,2.35789849937043,-1.95156391047391E-15));
#4904=CARTESIAN_POINT('Origin',(2.5,2.35789849937043,-1.95156391047391E-15));
#4905=CARTESIAN_POINT('Origin',(2.5,2.35789849937043,-1.95156391047391E-15));
#4906=CARTESIAN_POINT('Origin',(2.5,2.35789849937043,-1.95156391047391E-15));
#4907=CARTESIAN_POINT('',(0.,0.,0.));
#4908=CARTESIAN_POINT('Origin',(0.,0.,-25.0375057290932));
#4909=CARTESIAN_POINT('',(-2.5,-3.06161699786838E-16,-5.));
#4910=CARTESIAN_POINT('Origin',(0.,0.,-5.));
#4911=CARTESIAN_POINT('',(-2.5,-3.06161699786838E-16,-4.9746));
#4912=CARTESIAN_POINT('',(-2.5,-3.06161699786838E-16,-25.0375057290932));
#4913=CARTESIAN_POINT('',(2.5,3.06161699786838E-16,-4.9746));
#4914=CARTESIAN_POINT('Origin',(0.,0.,-4.9746));
#4915=CARTESIAN_POINT('Origin',(0.,0.,-4.9746));
#4916=CARTESIAN_POINT('Origin',(0.,0.,-4.9746));
#4917=CARTESIAN_POINT('',(-2.1,2.57175827820944E-16,-4.69451698471611));
#4918=CARTESIAN_POINT('',(2.1,-2.57175827820944E-16,-4.69451698471611));
#4919=CARTESIAN_POINT('Origin',(0.,0.,-4.69451698471611));
#4920=CARTESIAN_POINT('',(2.5,-3.06161699786838E-16,-4.9746));
#4921=CARTESIAN_POINT('Origin',(0.,0.,-4.69451698471611));
#4922=CARTESIAN_POINT('Origin',(0.,0.,-0.308091316812274));
#4923=CARTESIAN_POINT('',(-2.1,-2.57175827820944E-16,-0.280083015283885));
#4924=CARTESIAN_POINT('Origin',(0.,0.,-0.280083015283884));
#4925=CARTESIAN_POINT('',(-2.5,-3.06161699786838E-16,3.71230823859037E-15));
#4926=CARTESIAN_POINT('',(-2.06,-2.52277240624355E-16,-0.308091316812274));
#4927=CARTESIAN_POINT('Origin',(0.,0.,3.46944695195361E-15));
#4928=CARTESIAN_POINT('Origin',(0.,0.,-4.));
#4929=CARTESIAN_POINT('',(-5.56078137864558,6.80999311611651E-16,-4.));
#4930=CARTESIAN_POINT('',(5.56078137864557,-6.80999311611651E-16,-4.));
#4931=CARTESIAN_POINT('Origin',(0.,0.,-4.));
#4932=CARTESIAN_POINT('',(4.19739386533236,-1.63989485852606E-11,-3.5037678126099));
#4933=CARTESIAN_POINT('',(5.56078137864557,-6.80999311611651E-16,-4.));
#4934=CARTESIAN_POINT('',(4.21114047113378,-2.43130308459281,-3.74588532543563));
#4935=CARTESIAN_POINT('Ctrl Pts',(4.1973939570023,7.7729029084661E-14,-3.50376756074893));
#4936=CARTESIAN_POINT('Ctrl Pts',(4.1973939570023,-0.406987107455746,-3.50376756074893));
#4937=CARTESIAN_POINT('Ctrl Pts',(4.19892854886077,-0.815883880986012,-3.52647143761692));
#4938=CARTESIAN_POINT('Ctrl Pts',(4.20401592436619,-1.62672484819093,-3.61062719041339));
#4939=CARTESIAN_POINT('Ctrl Pts',(4.20749145004057,-2.02981982514649,-3.67167082875957));
#4940=CARTESIAN_POINT('Ctrl Pts',(4.2111405601822,-2.43130313601656,-3.74588504288744));
#4941=CARTESIAN_POINT('',(7.14602004806277E-12,-4.86260614339647,-3.74588539632542));
#4942=CARTESIAN_POINT('Ctrl Pts',(4.21114036026457,-2.4313030205652,-3.74588567721715));
#4943=CARTESIAN_POINT('Ctrl Pts',(4.01254994076142,-2.54356158437356,-3.70372906392697));
#4944=CARTESIAN_POINT('Ctrl Pts',(3.81342725369011,-2.65620468295633,-3.66594310691183));
#4945=CARTESIAN_POINT('Ctrl Pts',(3.61393376345345,-2.7692906630002,-3.63348439979832));
#4946=CARTESIAN_POINT('Ctrl Pts',(3.42914532611981,-2.87404085565993,-3.60341828707324));
#4947=CARTESIAN_POINT('Ctrl Pts',(3.24403860215133,-2.97917130976551,-3.577923704644));
#4948=CARTESIAN_POINT('Ctrl Pts',(3.05874390643497,-3.08472586676541,-3.55771928043663));
#4949=CARTESIAN_POINT('Ctrl Pts',(2.88773569998093,-3.18214201462554,-3.53907264658248));
#4950=CARTESIAN_POINT('Ctrl Pts',(2.71656732320876,-3.27991952009122,-3.52493209277403));
#4951=CARTESIAN_POINT('Ctrl Pts',(2.54534428121679,-3.37808801310675,-3.51581971997351));
#4952=CARTESIAN_POINT('Ctrl Pts',(2.39699951098393,-3.46313954805832,-3.5079249130968));
#4953=CARTESIAN_POINT('Ctrl Pts',(2.24861371330972,-3.54848456051724,-3.50380398528744));
#4954=CARTESIAN_POINT('Ctrl Pts',(2.10025818716125,-3.63413792844054,-3.50376507030381));
#4955=CARTESIAN_POINT('Ctrl Pts',(2.0947836520027,-3.63729866256564,-3.50376363428419));
#4956=CARTESIAN_POINT('Ctrl Pts',(2.08930702825758,-3.64046099613376,-3.50376773690171));
#4957=CARTESIAN_POINT('Ctrl Pts',(2.08382833422878,-3.64362492389969,-3.50377740609618));
#4958=CARTESIAN_POINT('Ctrl Pts',(1.96293505333574,-3.71344039563817,-3.5039907672798));
#4959=CARTESIAN_POINT('Ctrl Pts',(1.84199090601466,-3.78347495065613,-3.5068800488842));
#4960=CARTESIAN_POINT('Ctrl Pts',(1.72115880571068,-3.85362529081441,-3.51232413713592));
#4961=CARTESIAN_POINT('Ctrl Pts',(1.59475077179073,-3.92701279757723,-3.51801944898314));
#4962=CARTESIAN_POINT('Ctrl Pts',(1.46846525155069,-4.00052698685701,-3.52651072880892));
#4963=CARTESIAN_POINT('Ctrl Pts',(1.34247226888016,-4.07405414400108,-3.53760308570294));
#4964=CARTESIAN_POINT('Ctrl Pts',(1.24270876420383,-4.13227426650394,-3.5463862129487));
#4965=CARTESIAN_POINT('Ctrl Pts',(1.14312828434623,-4.19050262268746,-3.55679891920022));
#4966=CARTESIAN_POINT('Ctrl Pts',(1.04380946022049,-4.24868470200342,-3.5687222525591));
#4967=CARTESIAN_POINT('Ctrl Pts',(0.864208532035138,-4.35389693685298,-3.59028354023209));
#4968=CARTESIAN_POINT('Ctrl Pts',(0.685256950144924,-4.45903161754731,-3.61679277506933));
#4969=CARTESIAN_POINT('Ctrl Pts',(0.506826534709686,-4.56402874599945,-3.64753780817784));
#4970=CARTESIAN_POINT('Ctrl Pts',(0.337456180068921,-4.66369449434636,-3.67672171804169));
#4971=CARTESIAN_POINT('Ctrl Pts',(0.168554912827431,-4.76323644283656,-3.7097209642112));
#4972=CARTESIAN_POINT('Ctrl Pts',(5.49614199430651E-12,-4.86260619450716,
-3.7458852558793));
#4973=CARTESIAN_POINT('',(-4.21114045006265,-2.43130307244757,-3.74588539224308));
#4974=CARTESIAN_POINT('Ctrl Pts',(1.79620807498344E-11,-4.86260604116954,
-3.74588567721565));
#4975=CARTESIAN_POINT('Ctrl Pts',(-0.196513977808605,-4.74675097482129,
-3.7037290639203));
#4976=CARTESIAN_POINT('Ctrl Pts',(-0.393627106302676,-4.63062721862453,
-3.66594310690113));
#4977=CARTESIAN_POINT('Ctrl Pts',(-0.591309182975744,-4.51440377819733,
-3.63348439978504));
#4978=CARTESIAN_POINT('Ctrl Pts',(-0.774419729558393,-4.40674739345823,
-3.60341828705788));
#4979=CARTESIAN_POINT('Ctrl Pts',(-0.958018735530767,-4.2990054951306,-3.57792370462771));
#4980=CARTESIAN_POINT('Ctrl Pts',(-1.14207901125747,-4.19131285994132,-3.55771928042079));
#4981=CARTESIAN_POINT('Ctrl Pts',(-1.31194797329025,-4.09192348281499,-3.53907264656702));
#4982=CARTESIAN_POINT('Ctrl Pts',(-1.48220996534842,-3.99257607292704,-3.52493209276015));
#4983=CARTESIAN_POINT('Ctrl Pts',(-1.65283789516731,-3.89337681534504,-3.51581971996257));
#4984=CARTESIAN_POINT('Ctrl Pts',(-1.80066707011438,-3.80743224332055,-3.507924913093));
#4985=CARTESIAN_POINT('Ctrl Pts',(-1.94877091775868,-3.72159887924319,-3.50380398528742));
#4986=CARTESIAN_POINT('Ctrl Pts',(-2.09712667330543,-3.63594590880816,-3.5037650703038));
#4987=CARTESIAN_POINT('Ctrl Pts',(-2.10260121693164,-3.6327851893495,-3.50376363428419));
#4988=CARTESIAN_POINT('Ctrl Pts',(-2.10807819000943,-3.62962346084331,-3.5037677369017));
#4989=CARTESIAN_POINT('Ctrl Pts',(-2.11355757884486,-3.62646073651777,-3.50377740609617));
#4990=CARTESIAN_POINT('Ctrl Pts',(-2.23446619139723,-3.55667181998499,-3.5039907672798));
#4991=CARTESIAN_POINT('Ctrl Pts',(-2.35558996884922,-3.48694839347305,-3.50688004888436));
#4992=CARTESIAN_POINT('Ctrl Pts',(-2.47675799566555,-3.41737989509451,-3.51232413713636));
#4993=CARTESIAN_POINT('Ctrl Pts',(-2.60351745780718,-3.34460107985613,-3.51801944898395));
#4994=CARTESIAN_POINT('Ctrl Pts',(-2.73032537338674,-3.27199170583537,-3.52651072881029));
#4995=CARTESIAN_POINT('Ctrl Pts',(-2.85699825068146,-3.19964216071353,-3.53760308570505));
#4996=CARTESIAN_POINT('Ctrl Pts',(-2.95730010811074,-3.14235449254917,-3.54638621295039));
#4997=CARTESIAN_POINT('Ctrl Pts',(-3.05751758370728,-3.08522944536764,-3.55679891920123));
#4998=CARTESIAN_POINT('Ctrl Pts',(-3.157564154495,-3.02830786026315,-3.56872225255918));
#4999=CARTESIAN_POINT('Ctrl Pts',(-3.33848108677305,-2.92537501132664,-3.59028354023417));
#5000=CARTESIAN_POINT('Ctrl Pts',(-3.51900618203487,-2.82296573570007,-3.6167927750743));
#5001=CARTESIAN_POINT('Ctrl Pts',(-3.69915157033305,-2.72093902734208,-3.64753780818642));
#5002=CARTESIAN_POINT('Ctrl Pts',(-3.87014981759516,-2.62409287175656,-3.67672171804863));
#5003=CARTESIAN_POINT('Ctrl Pts',(-4.04080630733679,-2.52759105784699,-3.70972096421582));
#5004=CARTESIAN_POINT('Ctrl Pts',(-4.21114049304847,-2.43130309725362,-3.7458852558811));
#5005=CARTESIAN_POINT('',(-4.19739387007612,1.49812671196668E-11,-3.50376779957655));
#5006=CARTESIAN_POINT('Ctrl Pts',(-4.21114036409982,-2.43130302282868,-3.7458856649686));
#5007=CARTESIAN_POINT('Ctrl Pts',(-4.20908206342616,-2.20517585842347,-3.70409596729133));
#5008=CARTESIAN_POINT('Ctrl Pts',(-4.20708960517473,-1.97840718425451,-3.66659889897082));
#5009=CARTESIAN_POINT('Ctrl Pts',(-4.20529095013208,-1.75110446615803,-3.63432933778681));
#5010=CARTESIAN_POINT('Ctrl Pts',(-4.2036243969318,-1.54049594852025,-3.6044298077561));
#5011=CARTESIAN_POINT('Ctrl Pts',(-4.20212438692378,-1.32942868276544,-3.57901881382086));
#5012=CARTESIAN_POINT('Ctrl Pts',(-4.20089156122566,-1.11799092190762,-3.55879847693247));
#5013=CARTESIAN_POINT('Ctrl Pts',(-4.19975422779664,-0.922930716764744,
-3.54014436782016));
#5014=CARTESIAN_POINT('Ctrl Pts',(-4.19884437084874,-0.727555053652698,
-3.52590816900496));
#5015=CARTESIAN_POINT('Ctrl Pts',(-4.1982384076207,-0.531938318567338,-3.51659854639054));
#5016=CARTESIAN_POINT('Ctrl Pts',(-4.1976896945174,-0.354803039069626,-3.50816847723974));
#5017=CARTESIAN_POINT('Ctrl Pts',(-4.19739018650638,-0.177470047501419,
-3.50377792009247));
#5018=CARTESIAN_POINT('Ctrl Pts',(-4.19739378314994,3.00402705630902E-11,
-3.50376803840416));
#5019=CARTESIAN_POINT('',(-4.21114047113314,2.43130308459242,-3.74588532543767));
#5020=CARTESIAN_POINT('Ctrl Pts',(-4.1973939570023,-7.77393595236366E-14,
-3.50376756074893));
#5021=CARTESIAN_POINT('Ctrl Pts',(-4.1973939570023,0.406987107455743,-3.50376756074893));
#5022=CARTESIAN_POINT('Ctrl Pts',(-4.19892854886077,0.815883880986007,-3.52647143761692));
#5023=CARTESIAN_POINT('Ctrl Pts',(-4.20401592436619,1.62672484819092,-3.61062719041339));
#5024=CARTESIAN_POINT('Ctrl Pts',(-4.20749145004057,2.02981982514647,-3.67167082875957));
#5025=CARTESIAN_POINT('Ctrl Pts',(-4.2111405601822,2.43130313601654,-3.74588504288743));
#5026=CARTESIAN_POINT('',(-9.51175986589573E-12,4.86260614339766,-3.74588539632585));
#5027=CARTESIAN_POINT('Ctrl Pts',(-4.21114036026505,2.43130302056491,-3.74588567721725));
#5028=CARTESIAN_POINT('Ctrl Pts',(-4.01254994075699,2.54356158437606,-3.70372906392602));
#5029=CARTESIAN_POINT('Ctrl Pts',(-3.81342725368073,2.65620468296162,-3.66594310691005));
#5030=CARTESIAN_POINT('Ctrl Pts',(-3.61393376343911,2.76929066300832,-3.633484399796));
#5031=CARTESIAN_POINT('Ctrl Pts',(-3.42914532610122,2.87404085567046,-3.60341828707046));
#5032=CARTESIAN_POINT('Ctrl Pts',(-3.24403860212847,2.97917130977849,-3.57792370464101));
#5033=CARTESIAN_POINT('Ctrl Pts',(-3.05874390640785,3.08472586678085,-3.55771928043369));
#5034=CARTESIAN_POINT('Ctrl Pts',(-2.88773569994925,3.18214201464361,-3.53907264657952));
#5035=CARTESIAN_POINT('Ctrl Pts',(-2.71656732317253,3.27991952011193,-3.52493209277131));
#5036=CARTESIAN_POINT('Ctrl Pts',(-2.54534428117601,3.37808801313014,-3.51581971997135));
#5037=CARTESIAN_POINT('Ctrl Pts',(-2.39699951095675,3.46313954807398,-3.50792491309605));
#5038=CARTESIAN_POINT('Ctrl Pts',(-2.24861371329614,3.5484845605251,-3.50380398528744));
#5039=CARTESIAN_POINT('Ctrl Pts',(-2.10025818716127,3.63413792844057,-3.50376507030382));
#5040=CARTESIAN_POINT('Ctrl Pts',(-2.09478365200272,3.63729866256567,-3.5037636342842));
#5041=CARTESIAN_POINT('Ctrl Pts',(-2.0893070282576,3.64046099613379,-3.50376773690172));
#5042=CARTESIAN_POINT('Ctrl Pts',(-2.0838283342288,3.64362492389971,-3.50377740609619));
#5043=CARTESIAN_POINT('Ctrl Pts',(-1.96293505333605,3.71344039563804,-3.50399076727982));
#5044=CARTESIAN_POINT('Ctrl Pts',(-1.84199090601524,3.78347495065584,-3.5068800488842));
#5045=CARTESIAN_POINT('Ctrl Pts',(-1.72115880571154,3.85362529081395,-3.51232413713589));
#5046=CARTESIAN_POINT('Ctrl Pts',(-1.59475077179095,3.92701279757712,-3.51801944898313));
#5047=CARTESIAN_POINT('Ctrl Pts',(-1.46846525155029,4.00052698685725,-3.52651072880895));
#5048=CARTESIAN_POINT('Ctrl Pts',(-1.34247226887913,4.07405414400167,-3.53760308570303));
#5049=CARTESIAN_POINT('Ctrl Pts',(-1.24270876420315,4.13227426650433,-3.54638621294877));
#5050=CARTESIAN_POINT('Ctrl Pts',(-1.14312828434588,4.19050262268764,-3.55679891920027));
#5051=CARTESIAN_POINT('Ctrl Pts',(-1.04380946022048,4.2486847020034,-3.56872225255911));
#5052=CARTESIAN_POINT('Ctrl Pts',(-0.864208532033562,4.35389693685388,-3.59028354023228));
#5053=CARTESIAN_POINT('Ctrl Pts',(-0.685256950141792,4.45903161754913,-3.61679277506979));
#5054=CARTESIAN_POINT('Ctrl Pts',(-0.506826534705005,4.56402874600219,-3.64753780817865));
#5055=CARTESIAN_POINT('Ctrl Pts',(-0.337456180063016,4.66369449434982,-3.67672171804278));
#5056=CARTESIAN_POINT('Ctrl Pts',(-0.1685549128203,4.76323644284074,-3.70972096421261));
#5057=CARTESIAN_POINT('Ctrl Pts',(2.85244410943447E-12,4.86260619451207,
-3.74588525588108));
#5058=CARTESIAN_POINT('',(4.21114044751304,2.43130307097638,-3.74588540033132));
#5059=CARTESIAN_POINT('Ctrl Pts',(-2.02518052867876E-11,4.86260604117087,
-3.74588567721613));
#5060=CARTESIAN_POINT('Ctrl Pts',(0.19651397780476,4.74675097482353,-3.70372906392109));
#5061=CARTESIAN_POINT('Ctrl Pts',(0.393627106297267,4.63062721862769,-3.66594310690214));
#5062=CARTESIAN_POINT('Ctrl Pts',(0.591309182968762,4.51440377820141,-3.63348439978618));
#5063=CARTESIAN_POINT('Ctrl Pts',(0.774419729549811,4.40674739346324,-3.60341828705915));
#5064=CARTESIAN_POINT('Ctrl Pts',(0.958018735520578,4.29900549513656,-3.57792370462905));
#5065=CARTESIAN_POINT('Ctrl Pts',(1.14207901124566,4.19131285994821,-3.55771928042208));
#5066=CARTESIAN_POINT('Ctrl Pts',(1.31194797327675,4.09192348282286,-3.53907264656829));
#5067=CARTESIAN_POINT('Ctrl Pts',(1.48220996533321,3.9925760729359,-3.52493209276128));
#5068=CARTESIAN_POINT('Ctrl Pts',(1.65283789515039,3.89337681535487,-3.51581971996347));
#5069=CARTESIAN_POINT('Ctrl Pts',(1.80066707010309,3.8074322433271,-3.50792491309331));
#5070=CARTESIAN_POINT('Ctrl Pts',(1.94877091775302,3.72159887924647,-3.50380398528742));
#5071=CARTESIAN_POINT('Ctrl Pts',(2.09712667330543,3.63594590880817,-3.50376507030381));
#5072=CARTESIAN_POINT('Ctrl Pts',(2.10260121693165,3.63278518934951,-3.50376363428419));
#5073=CARTESIAN_POINT('Ctrl Pts',(2.10807819000944,3.62962346084332,-3.50376773690171));
#5074=CARTESIAN_POINT('Ctrl Pts',(2.11355757884487,3.62646073651778,-3.50377740609618));
#5075=CARTESIAN_POINT('Ctrl Pts',(2.23446619139685,3.55667181998522,-3.50399076727981));
#5076=CARTESIAN_POINT('Ctrl Pts',(2.35558996884845,3.48694839347351,-3.50688004888434));
#5077=CARTESIAN_POINT('Ctrl Pts',(2.47675799566439,3.41737989509519,-3.51232413713631));
#5078=CARTESIAN_POINT('Ctrl Pts',(2.60351745780486,3.34460107985747,-3.51801944898383));
#5079=CARTESIAN_POINT('Ctrl Pts',(2.73032537338327,3.27199170583736,-3.52651072881004));
#5080=CARTESIAN_POINT('Ctrl Pts',(2.85699825067684,3.19964216071616,-3.53760308570463));
#5081=CARTESIAN_POINT('Ctrl Pts',(2.95730010810766,3.14235449255091,-3.54638621295005));
#5082=CARTESIAN_POINT('Ctrl Pts',(3.05751758370574,3.0852294453685,-3.55679891920103));
#5083=CARTESIAN_POINT('Ctrl Pts',(3.157564154495,3.02830786026314,-3.56872225255917));
#5084=CARTESIAN_POINT('Ctrl Pts',(3.33848108677087,2.92537501132787,-3.59028354023389));
#5085=CARTESIAN_POINT('Ctrl Pts',(3.51900618203053,2.82296573570252,-3.61679277507365));
#5086=CARTESIAN_POINT('Ctrl Pts',(3.69915157032656,2.72093902734574,-3.6475378081853));
#5087=CARTESIAN_POINT('Ctrl Pts',(3.87014981758778,2.62409287176072,-3.67672171804727));
#5088=CARTESIAN_POINT('Ctrl Pts',(4.04080630732854,2.52759105785164,-3.70972096421418));
#5089=CARTESIAN_POINT('Ctrl Pts',(4.21114049303935,2.43130309725876,-3.74588525587916));
#5090=CARTESIAN_POINT('Ctrl Pts',(4.21114035645151,2.43130301841489,-3.74588568923342));
#5091=CARTESIAN_POINT('Ctrl Pts',(4.20904504440769,2.20112279744945,-3.70334735266769));
#5092=CARTESIAN_POINT('Ctrl Pts',(4.20701816094358,1.97027747715211,-3.66526171181474));
#5093=CARTESIAN_POINT('Ctrl Pts',(4.20519448587801,1.73888075176048,-3.63260836994925));
#5094=CARTESIAN_POINT('Ctrl Pts',(4.2035056635924,1.52459480025731,-3.60236959963146));
#5095=CARTESIAN_POINT('Ctrl Pts',(4.20199126981785,1.30983574967937,-3.57679014301546));
#5096=CARTESIAN_POINT('Ctrl Pts',(4.20075710188212,1.09469708220331,-3.55660623332013));
#5097=CARTESIAN_POINT('Ctrl Pts',(4.19961779997554,0.896095346621634,-3.53797378782187));
#5098=CARTESIAN_POINT('Ctrl Pts',(4.19871737958875,0.697169997202399,-3.52393953141141));
#5099=CARTESIAN_POINT('Ctrl Pts',(4.1981363871834,0.497999620803157,-3.51503969854886));
#5100=CARTESIAN_POINT('Ctrl Pts',(4.19765260282079,0.332153195431398,-3.50762893047509));
#5101=CARTESIAN_POINT('Ctrl Pts',(4.19739028041404,0.166136914123517,-3.50377766208245));
#5102=CARTESIAN_POINT('Ctrl Pts',(4.19739377366243,-3.28756114544519E-11,
-3.50376806447087));
#5103=CARTESIAN_POINT('Origin',(0.,0.,-4.));
#5104=CARTESIAN_POINT('Origin',(0.,0.,-4.48445439793712));
#5105=CARTESIAN_POINT('',(-5.38445439793712,-6.59405484358858E-16,-5.));
#5106=CARTESIAN_POINT('Origin',(-5.38445439793712,-6.59405484358858E-16,
-4.48445439793712));
#5107=CARTESIAN_POINT('Origin',(0.,0.,-5.));
#5108=CARTESIAN_POINT('Origin',(0.,0.,-5.));
#5109=CARTESIAN_POINT('',(-2.1,-2.57175827820944E-16,-5.));
#5110=CARTESIAN_POINT('Origin',(1.56747850547613E-15,4.61880215351701,-5.));
#5111=CARTESIAN_POINT('',(1.09700060671018E-7,4.61880068173267,-3.43332218935783));
#5112=CARTESIAN_POINT('',(1.73472347597681E-15,4.61880215351701,-0.5));
#5113=CARTESIAN_POINT('',(1.56747850547613E-15,4.61880215351701,-5.));
#5114=CARTESIAN_POINT('',(-4.00000000017049,2.30939825730392,-3.43332219680665));
#5115=CARTESIAN_POINT('Ctrl Pts',(-2.43977409528084E-6,4.61880074491278,
-3.4333119175934));
#5116=CARTESIAN_POINT('Ctrl Pts',(-0.16663428147485,4.52259580625129,-3.40020822163793));
#5117=CARTESIAN_POINT('Ctrl Pts',(-0.333219628702097,4.42641771117134,-3.37037814524522));
#5118=CARTESIAN_POINT('Ctrl Pts',(-0.499799729884962,4.33024264503938,-3.34429832550047));
#5119=CARTESIAN_POINT('Ctrl Pts',(-0.664211398942607,4.23531952377698,-3.31855799599827));
#5120=CARTESIAN_POINT('Ctrl Pts',(-0.82861798209483,4.14039933903518,-3.29647105632394));
#5121=CARTESIAN_POINT('Ctrl Pts',(-0.993047089653662,4.0454661498736,-3.27844793346592));
#5122=CARTESIAN_POINT('Ctrl Pts',(-1.15827103668867,3.95007405992818,-3.26033768801905));
#5123=CARTESIAN_POINT('Ctrl Pts',(-1.32351778079621,3.8546688081062,-3.24633089903767));
#5124=CARTESIAN_POINT('Ctrl Pts',(-1.48880246969282,3.75924164848933,-3.23679221713863));
#5125=CARTESIAN_POINT('Ctrl Pts',(-1.65408715858944,3.66381448887247,-3.22725353523959));
#5126=CARTESIAN_POINT('Ctrl Pts',(-1.81940985241266,3.56836538664265,-3.22218315324263));
#5127=CARTESIAN_POINT('Ctrl Pts',(-1.98477204010767,3.47289348249879,-3.22189077969918));
#5128=CARTESIAN_POINT('Ctrl Pts',(-1.98984970207412,3.46996189297828,-3.22188180198764));
#5129=CARTESIAN_POINT('Ctrl Pts',(-1.99492568895773,3.46703127056732,-3.22187739028159));
#5130=CARTESIAN_POINT('Ctrl Pts',(-2.00000000019057,3.46410161559385,-3.22187752539236));
#5131=CARTESIAN_POINT('Ctrl Pts',(-2.20332030962145,3.34671457952159,-3.22188293908513));
#5132=CARTESIAN_POINT('Ctrl Pts',(-2.40664181574471,3.22932685336206,-3.22920718089928));
#5133=CARTESIAN_POINT('Ctrl Pts',(-2.60996148300162,3.11194018873347,-3.24317060794845));
#5134=CARTESIAN_POINT('Ctrl Pts',(-2.73997359254122,3.03687766228887,-3.25209947661895));
#5135=CARTESIAN_POINT('Ctrl Pts',(-2.86998504929241,2.96181551273783,-3.26374198223858));
#5136=CARTESIAN_POINT('Ctrl Pts',(-2.99999613197012,2.88675357915622,-3.27790934942572));
#5137=CARTESIAN_POINT('Ctrl Pts',(-3.20876161260061,2.7662227727167,-3.30065861940469));
#5138=CARTESIAN_POINT('Ctrl Pts',(-3.41752306189258,2.64569429377157,-3.32992036801802));
#5139=CARTESIAN_POINT('Ctrl Pts',(-3.62629054976681,2.52516232844934,-3.36487326410363));
#5140=CARTESIAN_POINT('Ctrl Pts',(-3.75085541086908,2.45324477236037,-3.38572853563255));
#5141=CARTESIAN_POINT('Ctrl Pts',(-3.87542250422839,2.38132592747721,-3.40860890830996));
#5142=CARTESIAN_POINT('Ctrl Pts',(-3.99999468199604,2.30940414710952,-3.43333114741226));
#5143=CARTESIAN_POINT('',(-4.,2.3094010767585,-0.499999999999993));
#5144=CARTESIAN_POINT('',(-4.,2.3094010767585,-5.));
#5145=CARTESIAN_POINT('',(-2.00000000000001,3.46410161513775,0.));
#5146=CARTESIAN_POINT('Ctrl Pts',(-4.,2.3094010767585,-0.499999999999992));
#5147=CARTESIAN_POINT('Ctrl Pts',(-2.92820323027552,2.9282032302755,-1.16573417585641E-15));
#5148=CARTESIAN_POINT('Ctrl Pts',(-2.00000000000001,3.46410161513775,5.26836153967997E-16));
#5149=CARTESIAN_POINT('Ctrl Pts',(-2.00000000000001,3.46410161513775,5.26836153967997E-16));
#5150=CARTESIAN_POINT('Ctrl Pts',(-1.0717967697245,4.,2.26437397702801E-15));
#5151=CARTESIAN_POINT('Ctrl Pts',(1.41896768074064E-16,4.61880215351701,
-0.499999999999997));
#5152=CARTESIAN_POINT('Origin',(4.,2.3094010767585,-5.));
#5153=CARTESIAN_POINT('',(3.99999878025273,2.3094002216274,-3.43332248801257));
#5154=CARTESIAN_POINT('',(4.,2.30940107675852,-0.5));
#5155=CARTESIAN_POINT('',(4.,2.3094010767585,-5.));
#5156=CARTESIAN_POINT('Ctrl Pts',(3.9999975602259,2.30940248536273,-3.43331191759338));
#5157=CARTESIAN_POINT('Ctrl Pts',(3.83336571851849,2.40560742402807,-3.40020822163658));
#5158=CARTESIAN_POINT('Ctrl Pts',(3.66678037127137,2.50178551908899,-3.37037814524283));
#5159=CARTESIAN_POINT('Ctrl Pts',(3.50020027019235,2.5979605854162,-3.34429832549734));
#5160=CARTESIAN_POINT('Ctrl Pts',(3.33578860123532,2.6928837068724,-3.31855799599412));
#5161=CARTESIAN_POINT('Ctrl Pts',(3.17138201833244,2.78780389206561,-3.29647105631917));
#5162=CARTESIAN_POINT('Ctrl Pts',(3.00695291106838,2.88273708175725,-3.27844793346097));
#5163=CARTESIAN_POINT('Ctrl Pts',(2.84172896434559,2.97812917222605,-3.26033768801568));
#5164=CARTESIAN_POINT('Ctrl Pts',(2.67648222056708,3.07353442460049,-3.24633089903554));
#5165=CARTESIAN_POINT('Ctrl Pts',(2.51119753168713,3.16896158422877,-3.23679221713734));
#5166=CARTESIAN_POINT('Ctrl Pts',(2.34591284280719,3.26438874385705,-3.22725353523913));
#5167=CARTESIAN_POINT('Ctrl Pts',(2.18059014860371,3.35983784541075,-3.22218315324262));
#5168=CARTESIAN_POINT('Ctrl Pts',(2.01522796042752,3.45530974870371,-3.22189077969918));
#5169=CARTESIAN_POINT('Ctrl Pts',(2.01015029844606,3.45824133819823,-3.22188180198763));
#5170=CARTESIAN_POINT('Ctrl Pts',(2.00507431154748,3.46117196058322,-3.22187739028159));
#5171=CARTESIAN_POINT('Ctrl Pts',(2.00000000029971,3.46410161553084,-3.22187752539235));
#5172=CARTESIAN_POINT('Ctrl Pts',(1.79667969023904,3.58148865058546,-3.22188293908513));
#5173=CARTESIAN_POINT('Ctrl Pts',(1.59335818419909,3.69887637696245,-3.22920718090153));
#5174=CARTESIAN_POINT('Ctrl Pts',(1.39003851690507,3.81626304159993,-3.2431706079549));
#5175=CARTESIAN_POINT('Ctrl Pts',(1.26002640739368,3.89132556802023,-3.25209947662451));
#5176=CARTESIAN_POINT('Ctrl Pts',(1.1300149506759,3.96638771755598,-3.26374198224188));
#5177=CARTESIAN_POINT('Ctrl Pts',(1.00000386802987,4.0414496511193,-3.27790934942554));
#5178=CARTESIAN_POINT('Ctrl Pts',(0.791238387378459,4.16198045757089,-3.30065861940672));
#5179=CARTESIAN_POINT('Ctrl Pts',(0.582476938065581,4.2825089365281,-3.32992036802359));
#5180=CARTESIAN_POINT('Ctrl Pts',(0.373709450170437,4.4030409018624,-3.36487326411387));
#5181=CARTESIAN_POINT('Ctrl Pts',(0.249144589089073,4.4749584579393,-3.38572853563997));
#5182=CARTESIAN_POINT('Ctrl Pts',(0.124577495750671,4.54687730281039,-3.40860890831389));
#5183=CARTESIAN_POINT('Ctrl Pts',(5.31800394343307E-6,4.618799083166,-3.43333114741212));
#5184=CARTESIAN_POINT('',(2.00000000000001,3.46410161513775,0.));
#5185=CARTESIAN_POINT('Ctrl Pts',(4.82449011451827E-15,4.61880215351701,
-0.499999999999999));
#5186=CARTESIAN_POINT('Ctrl Pts',(1.0717967697245,4.,-1.11022302462516E-15));
#5187=CARTESIAN_POINT('Ctrl Pts',(2.00000000000001,3.46410161513775,-1.44879942341204E-15));
#5188=CARTESIAN_POINT('Ctrl Pts',(2.00000000000001,3.46410161513775,-1.44879942341204E-15));
#5189=CARTESIAN_POINT('Ctrl Pts',(2.92820323027551,2.92820323027551,-1.86623997575081E-15));
#5190=CARTESIAN_POINT('Ctrl Pts',(3.99999999999999,2.3094010767585,-0.499999999999988));
#5191=CARTESIAN_POINT('Origin',(4.,2.3094010767585,-5.));
#5192=CARTESIAN_POINT('',(3.99999867054726,-2.30940043459921,-3.43332219625534));
#5193=CARTESIAN_POINT('',(4.,-2.30940107675852,-0.5));
#5194=CARTESIAN_POINT('',(4.,-2.30940107675851,-5.));
#5195=CARTESIAN_POINT('Ctrl Pts',(4.,-2.30939825700977,-3.43331193230041));
#5196=CARTESIAN_POINT('Ctrl Pts',(4.,-2.11694957105523,-3.40020158541481));
#5197=CARTESIAN_POINT('Ctrl Pts',(3.99999999998634,-1.92455454067137,-3.37036624965622));
#5198=CARTESIAN_POINT('Ctrl Pts',(4.00000000010068,-1.73216556308653,-3.34428277264658));
#5199=CARTESIAN_POINT('Ctrl Pts',(4.00000000021354,-1.54228190072953,-3.31853895819436));
#5200=CARTESIAN_POINT('Ctrl Pts',(4.00000000048029,-1.35240410653802,-3.29645005892505));
#5201=CARTESIAN_POINT('Ctrl Pts',(4.00000000079391,-1.16250031290758,-3.27842669391039));
#5202=CARTESIAN_POINT('Ctrl Pts',(4.00000000110889,-0.971775122729002,-3.26032537189695));
#5203=CARTESIAN_POINT('Ctrl Pts',(4.00000000144109,-0.781023646483771,-3.2463250813576));
#5204=CARTESIAN_POINT('Ctrl Pts',(4.00000000145045,-0.590228413801205,-3.236790121837));
#5205=CARTESIAN_POINT('Ctrl Pts',(4.00000000145981,-0.399433181118639,-3.2272551623164));
#5206=CARTESIAN_POINT('Ctrl Pts',(4.00000000105901,-0.208594122424576,-3.22218572635334));
#5207=CARTESIAN_POINT('Ctrl Pts',(4.00000000055376,-0.0177094910373128,
-3.22189127571074));
#5208=CARTESIAN_POINT('Ctrl Pts',(4.00000000053813,-0.0118043805065834,
-3.2218821667344));
#5209=CARTESIAN_POINT('Ctrl Pts',(4.00000000052252,-0.0059012165529552,
-3.22187769126366));
#5210=CARTESIAN_POINT('Ctrl Pts',(4.00000000050698,-6.5066340334549E-11,
-3.2218778296733));
#5211=CARTESIAN_POINT('Ctrl Pts',(3.99999999987799,0.238764894989697,-3.22188342976665));
#5212=CARTESIAN_POINT('Ctrl Pts',(4.00000000000652,0.477530878358765,-3.22946180827315));
#5213=CARTESIAN_POINT('Ctrl Pts',(4.00000000000153,0.716294821461492,-3.24389360090326));
#5214=CARTESIAN_POINT('Ctrl Pts',(3.99999999999847,0.862428932159365,-3.25272649733801));
#5215=CARTESIAN_POINT('Ctrl Pts',(4.,1.00856237380136,-3.26412563955697));
#5216=CARTESIAN_POINT('Ctrl Pts',(4.,1.1546953597049,-3.27791652926043));
#5217=CARTESIAN_POINT('Ctrl Pts',(4.,1.3986057399827,-3.30093488566466));
#5218=CARTESIAN_POINT('Ctrl Pts',(4.,1.64251152018096,-3.33061880975289));
#5219=CARTESIAN_POINT('Ctrl Pts',(4.,1.88642485026101,-3.36611862393459));
#5220=CARTESIAN_POINT('Ctrl Pts',(4.,2.02741126626355,-3.38663817310639));
#5221=CARTESIAN_POINT('Ctrl Pts',(4.,2.16840027918935,-3.4090998642691));
#5222=CARTESIAN_POINT('Ctrl Pts',(4.,2.30939483911209,-3.43333170804235));
#5223=CARTESIAN_POINT('',(4.,0.,0.));
#5224=CARTESIAN_POINT('Ctrl Pts',(4.,-2.10734454975715E-15,2.63418068719643E-16));
#5225=CARTESIAN_POINT('Ctrl Pts',(4.,1.07179676972449,7.12431934417829E-16));
#5226=CARTESIAN_POINT('Ctrl Pts',(4.,2.3094010767585,-0.499999999999993));
#5227=CARTESIAN_POINT('Ctrl Pts',(4.,-2.30940107675851,-0.499999999999998));
#5228=CARTESIAN_POINT('Ctrl Pts',(4.,-1.0717967697245,-3.33066907387547E-16));
#5229=CARTESIAN_POINT('Ctrl Pts',(4.,-2.10734454975715E-15,2.63418068719643E-16));
#5230=CARTESIAN_POINT('Origin',(-6.25964416140486E-16,-4.61880215351703,
-5.));
#5231=CARTESIAN_POINT('',(-1.09700057365134E-7,-4.61880068173268,-3.43332218935784));
#5232=CARTESIAN_POINT('',(-2.68882138776405E-14,-4.61880215351701,-0.5));
#5233=CARTESIAN_POINT('',(-6.25964416140486E-16,-4.61880215351703,-5.));
#5234=CARTESIAN_POINT('Ctrl Pts',(2.43977409417062E-6,-4.6188007449128,
-3.43331191759339));
#5235=CARTESIAN_POINT('Ctrl Pts',(0.166634281473495,-4.52259580625208,-3.40020822163818));
#5236=CARTESIAN_POINT('Ctrl Pts',(0.333219628699384,-4.42641771117292,-3.37037814524569));
#5237=CARTESIAN_POINT('Ctrl Pts',(0.499799729880895,-4.33024264504174,-3.34429832550108));
#5238=CARTESIAN_POINT('Ctrl Pts',(0.664211398937362,-4.23531952378002,-3.318557995999));
#5239=CARTESIAN_POINT('Ctrl Pts',(0.828617982088412,-4.1403993390389,-3.29647105632474));
#5240=CARTESIAN_POINT('Ctrl Pts',(0.993047089646068,-4.045466149878,-3.27844793346673));
#5241=CARTESIAN_POINT('Ctrl Pts',(1.15827103668234,-3.95007405993185,-3.2603376880196));
#5242=CARTESIAN_POINT('Ctrl Pts',(1.32351778079115,-3.85466880810913,-3.24633089903802));
#5243=CARTESIAN_POINT('Ctrl Pts',(1.48880246968903,-3.75924164849154,-3.23679221713884));
#5244=CARTESIAN_POINT('Ctrl Pts',(1.65408715858691,-3.66381448887394,-3.22725353523966));
#5245=CARTESIAN_POINT('Ctrl Pts',(1.8194098524114,-3.56836538664339,-3.22218315324264));
#5246=CARTESIAN_POINT('Ctrl Pts',(1.98477204010769,-3.4728934824988,-3.22189077969918));
#5247=CARTESIAN_POINT('Ctrl Pts',(1.98984970207413,-3.46996189297829,-3.22188180198764));
#5248=CARTESIAN_POINT('Ctrl Pts',(1.99492568895772,-3.46703127056734,-3.2218773902816));
#5249=CARTESIAN_POINT('Ctrl Pts',(2.00000000019056,-3.46410161559387,-3.22187752539236));
#5250=CARTESIAN_POINT('Ctrl Pts',(2.203320309618,-3.3467145795236,-3.22188293908513));
#5251=CARTESIAN_POINT('Ctrl Pts',(2.40664181573781,-3.22932685336607,-3.22920718089901));
#5252=CARTESIAN_POINT('Ctrl Pts',(2.60996148299126,-3.11194018873947,-3.2431706079477));
#5253=CARTESIAN_POINT('Ctrl Pts',(2.73997359253431,-3.03687766229287,-3.25209947661828));
#5254=CARTESIAN_POINT('Ctrl Pts',(2.86998504928896,-2.96181551273984,-3.26374198223814));
#5255=CARTESIAN_POINT('Ctrl Pts',(2.99999613197013,-2.88675357915623,-3.27790934942565));
#5256=CARTESIAN_POINT('Ctrl Pts',(3.20876161259695,-2.76622277271884,-3.30065861940419));
#5257=CARTESIAN_POINT('Ctrl Pts',(3.41752306188524,-2.64569429377582,-3.32992036801689));
#5258=CARTESIAN_POINT('Ctrl Pts',(3.62629054975579,-2.52516232845572,-3.3648732641017));
#5259=CARTESIAN_POINT('Ctrl Pts',(3.75085541086174,-2.45324477236463,-3.38572853563112));
#5260=CARTESIAN_POINT('Ctrl Pts',(3.87542250422473,-2.38132592747934,-3.40860890830916));
#5261=CARTESIAN_POINT('Ctrl Pts',(3.99999468199605,-2.30940414710953,-3.43333114741222));
#5262=CARTESIAN_POINT('',(2.00000000000001,-3.46410161513775,0.));
#5263=CARTESIAN_POINT('Ctrl Pts',(4.,-2.30940107675852,-0.499999999999999));
#5264=CARTESIAN_POINT('Ctrl Pts',(2.92820323027552,-2.92820323027552,-1.2267964422108E-14));
#5265=CARTESIAN_POINT('Ctrl Pts',(2.00000000000001,-3.46410161513777,-1.21172315412642E-14));
#5266=CARTESIAN_POINT('Ctrl Pts',(2.00000000000001,-3.46410161513777,-1.21172315412642E-14));
#5267=CARTESIAN_POINT('Ctrl Pts',(1.0717967697245,-4.00000000000002,-1.21572333146255E-14));
#5268=CARTESIAN_POINT('Ctrl Pts',(-7.09483840370325E-16,-4.61880215351703,
-0.500000000000012));
#5269=CARTESIAN_POINT('Origin',(-4.,-2.30940107675851,-5.));
#5270=CARTESIAN_POINT('',(-3.99999878024205,-2.30940027055269,-3.43332188511301));
#5271=CARTESIAN_POINT('',(-4.,-2.30940107675852,-0.5));
#5272=CARTESIAN_POINT('',(-4.,-2.30940107675851,-5.));
#5273=CARTESIAN_POINT('Ctrl Pts',(-3.99999756022589,-2.30940248536275,-3.43331191759346));
#5274=CARTESIAN_POINT('Ctrl Pts',(-3.83336571851771,-2.40560742402853,-3.40020822163657));
#5275=CARTESIAN_POINT('Ctrl Pts',(-3.66678037126983,-2.50178551908989,-3.37037814524273));
#5276=CARTESIAN_POINT('Ctrl Pts',(-3.50020027019005,-2.59796058541755,-3.34429832549716));
#5277=CARTESIAN_POINT('Ctrl Pts',(-3.33578860123178,-2.69288370687446,-3.31855799599379));
#5278=CARTESIAN_POINT('Ctrl Pts',(-3.17138201832767,-2.78780389206838,-3.29647105631872));
#5279=CARTESIAN_POINT('Ctrl Pts',(-3.00695291106237,-2.88273708176073,-3.27844793346046));
#5280=CARTESIAN_POINT('Ctrl Pts',(-2.84172896434058,-2.97812917222895,-3.26033768801535));
#5281=CARTESIAN_POINT('Ctrl Pts',(-2.67648222056308,-3.07353442460281,-3.24633089903534));
#5282=CARTESIAN_POINT('Ctrl Pts',(-2.51119753168413,-3.16896158423052,-3.23679221713722));
#5283=CARTESIAN_POINT('Ctrl Pts',(-2.34591284280519,-3.26438874385822,-3.2272535352391));
#5284=CARTESIAN_POINT('Ctrl Pts',(-2.1805901486027,-3.35983784541135,-3.22218315324262));
#5285=CARTESIAN_POINT('Ctrl Pts',(-2.01522796042751,-3.45530974870373,-3.22189077969918));
#5286=CARTESIAN_POINT('Ctrl Pts',(-2.01015029844606,-3.45824133819825,-3.22188180198764));
#5287=CARTESIAN_POINT('Ctrl Pts',(-2.00507431154748,-3.46117196058324,-3.2218773902816));
#5288=CARTESIAN_POINT('Ctrl Pts',(-2.00000000029972,-3.46410161553085,-3.22187752539236));
#5289=CARTESIAN_POINT('Ctrl Pts',(-1.79667969023426,-3.58148865058824,-3.22188293908513));
#5290=CARTESIAN_POINT('Ctrl Pts',(-1.59335818418951,-3.69887637696799,-3.22920718090189));
#5291=CARTESIAN_POINT('Ctrl Pts',(-1.39003851689071,-3.81626304160823,-3.24317060795591));
#5292=CARTESIAN_POINT('Ctrl Pts',(-1.2600264073841,-3.89132556802577,-3.25209947662539));
#5293=CARTESIAN_POINT('Ctrl Pts',(-1.13001495067111,-3.96638771755876,-3.26374198224244));
#5294=CARTESIAN_POINT('Ctrl Pts',(-1.00000386802987,-4.04144965111931,-3.27790934942557));
#5295=CARTESIAN_POINT('Ctrl Pts',(-0.79123838737471,-4.16198045757307,-3.30065861940717));
#5296=CARTESIAN_POINT('Ctrl Pts',(-0.582476938058081,-4.28250893653244,
-3.32992036802469));
#5297=CARTESIAN_POINT('Ctrl Pts',(-0.373709450159184,-4.40304090186891,
-3.36487326411579));
#5298=CARTESIAN_POINT('Ctrl Pts',(-0.24914458908157,-4.47495845794364,-3.38572853564138));
#5299=CARTESIAN_POINT('Ctrl Pts',(-0.124577495746921,-4.54687730281257,
-3.40860890831466));
#5300=CARTESIAN_POINT('Ctrl Pts',(-5.31800394298898E-6,-4.61879908316602,
-3.43333114741214));
#5301=CARTESIAN_POINT('',(-2.00000000000001,-3.46410161513775,0.));
#5302=CARTESIAN_POINT('Ctrl Pts',(-2.7811766542517E-14,-4.61880215351701,
-0.499999999999999));
#5303=CARTESIAN_POINT('Ctrl Pts',(-1.07179676972451,-4.00000000000001,-1.11022302462516E-14));
#5304=CARTESIAN_POINT('Ctrl Pts',(-2.00000000000001,-3.46410161513776,-1.08001411563443E-14));
#5305=CARTESIAN_POINT('Ctrl Pts',(-2.00000000000001,-3.46410161513776,-1.08001411563443E-14));
#5306=CARTESIAN_POINT('Ctrl Pts',(-2.92820323027552,-2.92820323027552,-1.05539304160516E-14));
#5307=CARTESIAN_POINT('Ctrl Pts',(-4.00000000000001,-2.30940107675851,-0.500000000000001));
#5308=CARTESIAN_POINT('Origin',(-4.,2.3094010767585,-5.));
#5309=CARTESIAN_POINT('Ctrl Pts',(-4.,2.30939825683146,-3.43331193331253));
#5310=CARTESIAN_POINT('Ctrl Pts',(-4.,2.11697930046273,-3.40020670375471));
#5311=CARTESIAN_POINT('Ctrl Pts',(-3.99999999998728,1.9246139805551,-3.37037536084733));
#5312=CARTESIAN_POINT('Ctrl Pts',(-4.0000000000937,1.73225470564797,-3.34429462341928));
#5313=CARTESIAN_POINT('Ctrl Pts',(-4.00000000019874,1.54240087817937,-3.31855358324167));
#5314=CARTESIAN_POINT('Ctrl Pts',(-4.000000000447,1.352552910853,-3.29646621734035));
#5315=CARTESIAN_POINT('Ctrl Pts',(-4.00000000073897,1.16267895982991,-3.27844302243925));
#5316=CARTESIAN_POINT('Ctrl Pts',(-4.00000000103237,0.971876565599027,-3.26033169795114));
#5317=CARTESIAN_POINT('Ctrl Pts',(-4.00000000134192,0.781047869753778,-3.24632464433699));
#5318=CARTESIAN_POINT('Ctrl Pts',(-4.00000000135058,0.590175421017146,-3.23678664305403));
#5319=CARTESIAN_POINT('Ctrl Pts',(-4.00000000135925,0.399302972280514,-3.22724864177108));
#5320=CARTESIAN_POINT('Ctrl Pts',(-4.00000000098556,0.208386701389507,-3.2221798857123));
#5321=CARTESIAN_POINT('Ctrl Pts',(-4.00000000051493,0.017424937160016,-3.22189020190631));
#5322=CARTESIAN_POINT('Ctrl Pts',(-4.00000000050061,0.0116147111477252,
-3.22188138795137));
#5323=CARTESIAN_POINT('Ctrl Pts',(-4.00000000048631,0.00580639863921593,
-3.2218770559679));
#5324=CARTESIAN_POINT('Ctrl Pts',(-4.00000000047207,6.06586074236706E-11,
-3.22187718730854));
#5325=CARTESIAN_POINT('Ctrl Pts',(-3.99999999990536,-0.231030142290403,
-3.22188241320624));
#5326=CARTESIAN_POINT('Ctrl Pts',(-4.00000000000776,-0.462061954876961,
-3.22897203276302));
#5327=CARTESIAN_POINT('Ctrl Pts',(-4.00000000000194,-0.693091561426993,
-3.24250253777789));
#5328=CARTESIAN_POINT('Ctrl Pts',(-3.99999999999807,-0.846960671690658,
-3.25151405279168));
#5329=CARTESIAN_POINT('Ctrl Pts',(-4.,-1.00082893608218,-3.26338147840436));
#5330=CARTESIAN_POINT('Ctrl Pts',(-4.,-1.1546967992463,-3.27790201754606));
#5331=CARTESIAN_POINT('Ctrl Pts',(-4.,-1.39301162222072,-3.30039183214339));
#5332=CARTESIAN_POINT('Ctrl Pts',(-4.,-1.63132173464497,-3.32924825001008));
#5333=CARTESIAN_POINT('Ctrl Pts',(-4.,-1.86963826834349,-3.3636766457411));
#5334=CARTESIAN_POINT('Ctrl Pts',(-4.,-2.01622009482115,-3.38485258788254));
#5335=CARTESIAN_POINT('Ctrl Pts',(-4.,-2.16280446588197,-3.40813542735712));
#5336=CARTESIAN_POINT('Ctrl Pts',(-4.,-2.30939503481467,-3.43333057628833));
#5337=CARTESIAN_POINT('',(-4.,0.,0.));
#5338=CARTESIAN_POINT('Ctrl Pts',(-4.,-2.30940107675851,-0.499999999999998));
#5339=CARTESIAN_POINT('Ctrl Pts',(-4.,-1.07179676972449,1.33226762955019E-15));
#5340=CARTESIAN_POINT('Ctrl Pts',(-4.,2.1073447210992E-15,7.90254270412198E-16));
#5341=CARTESIAN_POINT('Ctrl Pts',(-4.,2.1073447210992E-15,7.90254270412198E-16));
#5342=CARTESIAN_POINT('Ctrl Pts',(-4.,1.07179676972449,2.71717901185061E-16));
#5343=CARTESIAN_POINT('Ctrl Pts',(-4.,2.3094010767585,-0.499999999999992));
#5344=CARTESIAN_POINT('Origin',(8.67361737988404E-16,4.61880215351701,0.));
#5345=CARTESIAN_POINT('Origin',(0.,0.,0.));
#5346=CARTESIAN_POINT('Origin',(0.,0.,0.));
#5347=CARTESIAN_POINT('Origin',(0.,0.,0.));
#5348=CARTESIAN_POINT('Origin',(0.,0.,0.));
#5349=CARTESIAN_POINT('Origin',(0.,0.,0.));
#5350=CARTESIAN_POINT('Origin',(0.,0.,0.));
#5351=CARTESIAN_POINT('Origin',(8.67361737988404E-16,4.61880215351701,-5.));
#5352=CARTESIAN_POINT('Origin',(0.,0.,0.));
#5353=CARTESIAN_POINT('Origin',(0.,0.,0.));
#5354=CARTESIAN_POINT('Origin',(0.,0.,0.));
#5355=CARTESIAN_POINT('Origin',(0.,0.,0.));
#5356=CARTESIAN_POINT('Origin',(0.,0.,0.));
#5357=CARTESIAN_POINT('Origin',(0.,0.,0.));
#5358=CARTESIAN_POINT('Ctrl Pts',(-4.17500251181215,-2.20836332945491,-3.46925408785825));
#5359=CARTESIAN_POINT('Ctrl Pts',(-4.14040488867328,-2.22833827648746,-3.68688706832704));
#5360=CARTESIAN_POINT('Ctrl Pts',(-4.23588660588939,-2.41731472804854,-3.75116187409402));
#5361=CARTESIAN_POINT('Ctrl Pts',(-3.47237194058605,-2.61402727889316,-3.32032231920216));
#5362=CARTESIAN_POINT('Ctrl Pts',(-3.4530385704595,-2.62518940534045,-3.53526375354527));
#5363=CARTESIAN_POINT('Ctrl Pts',(-3.54002001573559,-2.8106620929241,-3.60214640694581));
#5364=CARTESIAN_POINT('Ctrl Pts',(-2.75619783495007,-3.02751059156874,-3.22314629010981));
#5365=CARTESIAN_POINT('Ctrl Pts',(-2.74282792772311,-3.03522971110519,-3.4332526945506));
#5366=CARTESIAN_POINT('Ctrl Pts',(-2.8368931367585,-3.20894943574587,-3.50505407716489));
#5367=CARTESIAN_POINT('Ctrl Pts',(-1.27425813156503,-3.88310887824089,-3.22059942984405));
#5368=CARTESIAN_POINT('Ctrl Pts',(-1.28723743436171,-3.8756152742774,-3.43061871662682));
#5369=CARTESIAN_POINT('Ctrl Pts',(-1.39023091438237,-4.04398746048867,-3.50250721526052));
#5370=CARTESIAN_POINT('Ctrl Pts',(-0.544931331064667,-4.30418590283698,
-3.31662087526347));
#5371=CARTESIAN_POINT('Ctrl Pts',(-0.563680077012917,-4.29336130931743,
-3.53154229295521));
#5372=CARTESIAN_POINT('Ctrl Pts',(-0.68105971431977,-4.46107577825961,-3.59844171492072));
#5373=CARTESIAN_POINT('Ctrl Pts',(0.175648173966054,-4.720212674039,-3.46939095956407));
#5374=CARTESIAN_POINT('Ctrl Pts',(0.141042297810615,-4.70023296212511,-3.68702768697363));
#5375=CARTESIAN_POINT('Ctrl Pts',(0.0251197378185065,-4.87741561294743,
-3.75129874579984));
#5376=CARTESIAN_POINT('Ctrl Pts',(-4.21114049304847,-2.43130309725362,-3.7458852558811));
#5377=CARTESIAN_POINT('Ctrl Pts',(-4.18988746455481,-2.41903264520882,-3.73695337648562));
#5378=CARTESIAN_POINT('Ctrl Pts',(-4.16932200861515,-2.40716260740472,-3.72569031308385));
#5379=CARTESIAN_POINT('Ctrl Pts',(-4.14987580443041,-2.39594091351642,-3.71225681513601));
#5380=CARTESIAN_POINT('Ctrl Pts',(-4.13336582704669,-2.38641360882791,-3.7008516717365));
#5381=CARTESIAN_POINT('Ctrl Pts',(-4.11766043275974,-2.3773497008117,-3.68788163057286));
#5382=CARTESIAN_POINT('Ctrl Pts',(-4.10302583783635,-2.3688968958051,-3.67343984369392));
#5383=CARTESIAN_POINT('Ctrl Pts',(-4.08994531422733,-2.36134170783918,-3.66053165353114));
#5384=CARTESIAN_POINT('Ctrl Pts',(-4.07771995662713,-2.35427354186951,-3.64644578533102));
#5385=CARTESIAN_POINT('Ctrl Pts',(-4.0665555419278,-2.34782521054507,-3.6312629502672));
#5386=CARTESIAN_POINT('Ctrl Pts',(-4.06543294642031,-2.34717682296985,-3.62973629769359));
#5387=CARTESIAN_POINT('Ctrl Pts',(-4.0643210925777,-2.34653473372248,-3.62819858242172));
#5388=CARTESIAN_POINT('Ctrl Pts',(-4.06322019950523,-2.34589909973338,-3.62664990860538));
#5389=CARTESIAN_POINT('Ctrl Pts',(-4.05342647660366,-2.34024439691828,-3.61287265575376));
#5390=CARTESIAN_POINT('Ctrl Pts',(-4.04454702329777,-2.3351426055361,-3.59831218398053));
#5391=CARTESIAN_POINT('Ctrl Pts',(-4.03673870576888,-2.33065236670391,-3.58305397058372));
#5392=CARTESIAN_POINT('Ctrl Pts',(-4.02952082819937,-2.32650166534877,-3.56894953440778));
#5393=CARTESIAN_POINT('Ctrl Pts',(-4.02321878492448,-2.32287395117742,-3.55424736097336));
#5394=CARTESIAN_POINT('Ctrl Pts',(-4.01796736010047,-2.31984083523265,-3.53904370693992));
#5395=CARTESIAN_POINT('Ctrl Pts',(-4.01301173760937,-2.31697856868638,-3.52469644454925));
#5396=CARTESIAN_POINT('Ctrl Pts',(-4.00899243519024,-2.31464674979346,-3.50990175781935));
#5397=CARTESIAN_POINT('Ctrl Pts',(-4.00602358012327,-2.31291900655892,-3.49478367972883));
#5398=CARTESIAN_POINT('Ctrl Pts',(-4.00322852109713,-2.31129240498571,-3.480550610188));
#5399=CARTESIAN_POINT('Ctrl Pts',(-4.00136519487194,-2.31020233875389,-3.46603085078074));
#5400=CARTESIAN_POINT('Ctrl Pts',(-4.00051969176615,-2.30970772649789,-3.45137325050413));
#5401=CARTESIAN_POINT('Ctrl Pts',(-4.00017366263073,-2.3095053023434,-3.44537450642346));
#5402=CARTESIAN_POINT('Ctrl Pts',(-3.99999794474645,-2.30940248824816,-3.43935322510961));
#5403=CARTESIAN_POINT('Ctrl Pts',(-3.99999756070101,-2.30940248527412,-3.43332188518958));
#5404=CARTESIAN_POINT('Ctrl Pts',(2.43945024266171E-6,-4.61880074529696,
-3.4333221894343));
#5405=CARTESIAN_POINT('Ctrl Pts',(1.97908393093112E-6,-4.61880157394924,
-3.44798265290114));
#5406=CARTESIAN_POINT('Ctrl Pts',(1.01218396963414E-5,-4.62000512030333,
-3.4625805024101));
#5407=CARTESIAN_POINT('Ctrl Pts',(2.08731294980132E-5,-4.62231794296185,
-3.47695007304928));
#5408=CARTESIAN_POINT('Ctrl Pts',(3.2443490399229E-5,-4.62480696459119,
-3.49241436815785));
#5409=CARTESIAN_POINT('Ctrl Pts',(4.62192455342729E-5,-4.62857938934421,
-3.50761388627125));
#5410=CARTESIAN_POINT('Ctrl Pts',(5.292240897191E-5,-4.63349822781682,-3.52240062737015));
#5411=CARTESIAN_POINT('Ctrl Pts',(5.99895780237729E-5,-4.63868417671216,
-3.53799034109924));
#5412=CARTESIAN_POINT('Ctrl Pts',(5.84997758187179E-5,-4.64514293602618,
-3.55312199412916));
#5413=CARTESIAN_POINT('Ctrl Pts',(4.82387339152211E-5,-4.65271536558076,
-3.56768197579321));
#5414=CARTESIAN_POINT('Ctrl Pts',(3.67781382146205E-5,-4.66117304019241,
-3.58394407323217));
#5415=CARTESIAN_POINT('Ctrl Pts',(1.388586822648E-5,-4.67101852024403,-3.5994946447632));
#5416=CARTESIAN_POINT('Ctrl Pts',(3.07627714035774E-6,-4.6820576544963,
-3.61422980570673));
#5417=CARTESIAN_POINT('Ctrl Pts',(-1.12741608040529E-8,-4.68521077037762,
-3.6184386203586));
#5418=CARTESIAN_POINT('Ctrl Pts',(-1.95993311524184E-6,-4.68846149517478,
-3.62258112015053));
#5419=CARTESIAN_POINT('Ctrl Pts',(-1.88456980714909E-6,-4.6918058410115,
-3.62665524106977));
#5420=CARTESIAN_POINT('Ctrl Pts',(-1.59706231056096E-6,-4.70456436400585,
-3.64219782188156));
#5421=CARTESIAN_POINT('Ctrl Pts',(7.08251721277811E-6,-4.71861608899416,
-3.65664956360104));
#5422=CARTESIAN_POINT('Ctrl Pts',(1.08520660015016E-5,-4.73369614799714,
-3.66990623170299));
#5423=CARTESIAN_POINT('Ctrl Pts',(1.59548811295723E-5,-4.75410993158917,
-3.68785170219029));
#5424=CARTESIAN_POINT('Ctrl Pts',(1.26337967333387E-5,-4.77640804570073,
-3.70360921007672));
#5425=CARTESIAN_POINT('Ctrl Pts',(7.67272428404579E-6,-4.79999197504746,
-3.71699112236792));
#5426=CARTESIAN_POINT('Ctrl Pts',(3.4527694589582E-6,-4.8200527819513,-3.72837395660776));
#5427=CARTESIAN_POINT('Ctrl Pts',(-7.85645361820395E-9,-4.8410474613116,
-3.73803875904214));
#5428=CARTESIAN_POINT('Ctrl Pts',(-2.82044192924637E-12,-4.86260619451213,
-3.74588525588111));
#5429=CARTESIAN_POINT('Ctrl Pts',(-0.175002511812154,-4.71983990082064,
-3.46925408785825));
#5430=CARTESIAN_POINT('Ctrl Pts',(-0.14040488867328,-4.69986495378808,-3.68688706832704));
#5431=CARTESIAN_POINT('Ctrl Pts',(-0.0244873395123925,-4.87704277227474,
-3.75116187409403));
#5432=CARTESIAN_POINT('Ctrl Pts',(0.527628059414741,-4.31417595138192,-3.32032231920166));
#5433=CARTESIAN_POINT('Ctrl Pts',(0.546961429541539,-4.30301382493536,-3.53526375354356));
#5434=CARTESIAN_POINT('Ctrl Pts',(0.664094766059535,-4.47107830999418,-3.60214640694571));
#5435=CARTESIAN_POINT('Ctrl Pts',(1.24380216504877,-3.90069263870748,-3.22314629010981));
#5436=CARTESIAN_POINT('Ctrl Pts',(1.25717207227527,-3.89297351917098,-3.43325269455078));
#5437=CARTESIAN_POINT('Ctrl Pts',(1.36058516243511,-4.06129624212832,-3.50505407716491));
#5438=CARTESIAN_POINT('Ctrl Pts',(2.72574186843613,-3.04509435203399,-3.22059942984405));
#5439=CARTESIAN_POINT('Ctrl Pts',(2.71276256563965,-3.05258795599766,-3.43061871662663));
#5440=CARTESIAN_POINT('Ctrl Pts',(2.80708041617899,-3.22596901922515,-3.50250721526051));
#5441=CARTESIAN_POINT('Ctrl Pts',(3.45506866893442,-2.62401732743909,-3.31662087526373));
#5442=CARTESIAN_POINT('Ctrl Pts',(3.43631992298652,-2.63484192095947,-3.53154229295476));
#5443=CARTESIAN_POINT('Ctrl Pts',(3.52287509501949,-2.82035290322563,-3.59844171492057));
#5444=CARTESIAN_POINT('Ctrl Pts',(4.17564817396606,-2.20799055623655,-3.46939095956407));
#5445=CARTESIAN_POINT('Ctrl Pts',(4.14104229781062,-2.22797026815043,-3.68702768697362));
#5446=CARTESIAN_POINT('Ctrl Pts',(4.23652569453656,-2.41695347538648,-3.75129874579984));
#5447=CARTESIAN_POINT('Ctrl Pts',(4.00000000017051,-2.30939825748223,-3.43332219633194));
#5448=CARTESIAN_POINT('Ctrl Pts',(4.00000048725084,-2.30939907077008,-3.44798266367369));
#5449=CARTESIAN_POINT('Ctrl Pts',(4.00104686059629,-2.30999379289612,-3.46258051754916));
#5450=CARTESIAN_POINT('Ctrl Pts',(4.00305520041485,-2.31114089450209,-3.47695009281808));
#5451=CARTESIAN_POINT('Ctrl Pts',(4.00521654264325,-2.31237538635369,-3.49241439300576));
#5452=CARTESIAN_POINT('Ctrl Pts',(4.00849044815729,-2.31424967029535,-3.50761391649764));
#5453=CARTESIAN_POINT('Ctrl Pts',(4.01275364170441,-2.3167032865241,-3.52240066296025));
#5454=CARTESIAN_POINT('Ctrl Pts',(4.01724834205715,-2.31929014297502,-3.53799038315636));
#5455=CARTESIAN_POINT('Ctrl Pts',(4.02284105122292,-2.3225208156867,-3.55312204258641));
#5456=CARTESIAN_POINT('Ctrl Pts',(4.02939384253155,-2.32631592007399,-3.56768203020858));
#5457=CARTESIAN_POINT('Ctrl Pts',(4.0367126808535,-2.33055468705393,-3.58394413750869));
#5458=CARTESIAN_POINT('Ctrl Pts',(4.04522767987659,-2.33549725770526,-3.59949471806542));
#5459=CARTESIAN_POINT('Ctrl Pts',(4.05478245648888,-2.34102619219696,-3.6142298866834));
#5460=CARTESIAN_POINT('Ctrl Pts',(4.05751157529791,-2.34260541479184,-3.61843867433604));
#5461=CARTESIAN_POINT('Ctrl Pts',(4.06032579428629,-2.3442324549239,-3.62258114793907));
#5462=CARTESIAN_POINT('Ctrl Pts',(4.06322210246804,-2.34590455216165,-3.6266552435119));
#5463=CARTESIAN_POINT('Ctrl Pts',(4.07427144977102,-2.35228356362894,-3.64219782189265));
#5464=CARTESIAN_POINT('Ctrl Pts',(4.08644493860459,-2.35930190796122,-3.65664956136288));
#5465=CARTESIAN_POINT('Ctrl Pts',(4.09950653555256,-2.36683867144495,-3.66990622752824));
#5466=CARTESIAN_POINT('Ctrl Pts',(4.11718794719008,-2.37704114654056,-3.6878517032878));
#5467=CARTESIAN_POINT('Ctrl Pts',(4.13649702594183,-2.38819308295317,-3.70360921509657));
#5468=CARTESIAN_POINT('Ctrl Pts',(4.15691883376619,-2.39998934777108,-3.71699112998034));
#5469=CARTESIAN_POINT('Ctrl Pts',(4.17428988954401,-2.41002340429949,-3.72837396111162));
#5470=CARTESIAN_POINT('Ctrl Pts',(4.19247008180213,-2.42052373938338,-3.73803876108225));
#5471=CARTESIAN_POINT('Ctrl Pts',(4.21114049294513,-2.43130309720049,-3.74588525620001));
#5472=CARTESIAN_POINT('Ctrl Pts',(-4.,2.51147855358203,-3.46925445172476));
#5473=CARTESIAN_POINT('Ctrl Pts',(-4.,2.47152863417759,-3.68688744215519));
#5474=CARTESIAN_POINT('Ctrl Pts',(-4.21139928416427,2.45972999598821,-3.75116223796054));
#5475=CARTESIAN_POINT('Ctrl Pts',(-4.,1.70009491919674,-3.32031236430177));
#5476=CARTESIAN_POINT('Ctrl Pts',(-4.,1.67777237333276,-3.53525372389719));
#5477=CARTESIAN_POINT('Ctrl Pts',(-4.20411429709547,1.66036317409662,-3.60213643185789));
#5478=CARTESIAN_POINT('Ctrl Pts',(-4.,0.873073999173834,-3.22313462962843));
#5479=CARTESIAN_POINT('Ctrl Pts',(-4.,0.857636899345751,-3.4332406327822));
#5480=CARTESIAN_POINT('Ctrl Pts',(-4.19747753477223,0.852241327372437,-3.50504241668323));
#5481=CARTESIAN_POINT('Ctrl Pts',(-4.,-0.838224073004193,-3.22061061976714));
#5482=CARTESIAN_POINT('Ctrl Pts',(-4.,-0.823233910613052,-3.43063028686274));
#5483=CARTESIAN_POINT('Ctrl Pts',(-4.19731206413347,-0.818222978799002,
-3.50251840518389));
#5484=CARTESIAN_POINT('Ctrl Pts',(-4.,-1.68011768235794,-3.31661159321879));
#5485=CARTESIAN_POINT('Ctrl Pts',(-3.99999999999891,-1.65846997463859,-3.53153291307526));
#5486=CARTESIAN_POINT('Ctrl Pts',(-4.20393436246917,-1.64067374345485,-3.59843261460693));
#5487=CARTESIAN_POINT('Ctrl Pts',(-4.,-2.51222074532931,-3.46939070756972));
#5488=CARTESIAN_POINT('Ctrl Pts',(-4.,-2.47226133904334,-3.68702742808119));
#5489=CARTESIAN_POINT('Ctrl Pts',(-4.2114059444014,-2.46046078616939,-3.75129849380549));
#5490=CARTESIAN_POINT('Ctrl Pts',(-4.21114049294319,2.43130309719935,-3.74588525620613));
#5491=CARTESIAN_POINT('Ctrl Pts',(-4.18988744800146,2.41903265632003,-3.73695337399635));
#5492=CARTESIAN_POINT('Ctrl Pts',(-4.16932495849824,2.40715746377534,-3.72569030631416));
#5493=CARTESIAN_POINT('Ctrl Pts',(-4.14988357794915,2.39592740031508,-3.71225680267033));
#5494=CARTESIAN_POINT('Ctrl Pts',(-4.13337770500439,2.38639299507217,-3.70085166074699));
#5495=CARTESIAN_POINT('Ctrl Pts',(-4.11767543656294,2.37732368080158,-3.68788162176546));
#5496=CARTESIAN_POINT('Ctrl Pts',(-4.10303779813105,2.36887615430201,-3.67343983757684));
#5497=CARTESIAN_POINT('Ctrl Pts',(-4.08995455343392,2.36132568386283,-3.66053164905436));
#5498=CARTESIAN_POINT('Ctrl Pts',(-4.07772066494259,2.35427229783089,-3.64644578275999));
#5499=CARTESIAN_POINT('Ctrl Pts',(-4.06655404023516,2.34782779780516,-3.63126294971765));
#5500=CARTESIAN_POINT('Ctrl Pts',(-4.06543122325348,2.34717979590156,-3.62973629836));
#5501=CARTESIAN_POINT('Ctrl Pts',(-4.06431923159962,2.3465379473787,-3.62819858431993));
#5502=CARTESIAN_POINT('Ctrl Pts',(-4.06321831073147,2.34590236352179,-3.62664991175086));
#5503=CARTESIAN_POINT('Ctrl Pts',(-4.05342432406475,2.3402480971705,-3.61287264679811));
#5504=CARTESIAN_POINT('Ctrl Pts',(-4.0445663092799,2.33510915669676,-3.59831216137955));
#5505=CARTESIAN_POINT('Ctrl Pts',(-4.03677348473163,2.33059207189997,-3.58305393336723));
#5506=CARTESIAN_POINT('Ctrl Pts',(-4.0295699301827,2.32641655549583,-3.56894948675407));
#5507=CARTESIAN_POINT('Ctrl Pts',(-4.0232772145443,2.3227726820216,-3.55424730231654));
#5508=CARTESIAN_POINT('Ctrl Pts',(-4.0180247471138,2.31974137256816,-3.53904363726008));
#5509=CARTESIAN_POINT('Ctrl Pts',(-4.01306814118424,2.31688081101113,-3.52469636574108));
#5510=CARTESIAN_POINT('Ctrl Pts',(-4.00903907788616,2.31456590326902,-3.5099016699489));
#5511=CARTESIAN_POINT('Ctrl Pts',(-4.0060583845751,2.31285867251372,-3.49478358336693));
#5512=CARTESIAN_POINT('Ctrl Pts',(-4.00325218017958,2.31125138254802,-3.48055050515637));
#5513=CARTESIAN_POINT('Ctrl Pts',(-4.0013764967891,2.31018272987839,-3.466030737562));
#5514=CARTESIAN_POINT('Ctrl Pts',(-4.00052540443089,2.30969781163208,-3.45137313002631));
#5515=CARTESIAN_POINT('Ctrl Pts',(-4.00017709632775,2.30949935966277,-3.44537452901903));
#5516=CARTESIAN_POINT('Ctrl Pts',(-4.00000020054081,2.3093985918993,-3.43935339203637));
#5517=CARTESIAN_POINT('Ctrl Pts',(-4.00000000017049,2.30939825730392,-3.43332219680665));
#5518=CARTESIAN_POINT('Ctrl Pts',(4.,-2.51147557650728,-3.46925390523664));
#5519=CARTESIAN_POINT('Ctrl Pts',(4.,-2.47152569515979,-3.68688688070577));
#5520=CARTESIAN_POINT('Ctrl Pts',(4.21139925744971,-2.45972706465252,-3.75116169147242));
#5521=CARTESIAN_POINT('Ctrl Pts',(4.,-1.70017543050729,-3.32032727503766));
#5522=CARTESIAN_POINT('Ctrl Pts',(4.,-1.6778503894312,-3.53526875834698));
#5523=CARTESIAN_POINT('Ctrl Pts',(4.20411502351679,-1.6604426695002,-3.60215138177456));
#5524=CARTESIAN_POINT('Ctrl Pts',(4.,-0.873247063144998,-3.22315549424076));
#5525=CARTESIAN_POINT('Ctrl Pts',(4.,-0.857808282953852,-3.43326221544981));
#5526=CARTESIAN_POINT('Ctrl Pts',(4.19747890258699,-0.852410278374835,-3.5050632812955));
#5527=CARTESIAN_POINT('Ctrl Pts',(4.,0.837828026423296,-3.22059060139564));
#5528=CARTESIAN_POINT('Ctrl Pts',(4.,0.822843528041621,-3.43060958814149));
#5529=CARTESIAN_POINT('Ctrl Pts',(4.19731075179729,0.817836398951625,-3.50249838681244));
#5530=CARTESIAN_POINT('Ctrl Pts',(4.,1.68022822914713,-3.31663178303255));
#5531=CARTESIAN_POINT('Ctrl Pts',(4.00000000000109,1.65857727852441,-3.53155330955454));
#5532=CARTESIAN_POINT('Ctrl Pts',(4.20393533543406,1.64078067129417,-3.5984524478792));
#5533=CARTESIAN_POINT('Ctrl Pts',(4.,2.51222311093255,-3.4693911419088));
#5534=CARTESIAN_POINT('Ctrl Pts',(4.,2.47226367441142,-3.68702787430986));
#5535=CARTESIAN_POINT('Ctrl Pts',(4.21140596563046,2.46046311543628,-3.75129892814458));
#5536=CARTESIAN_POINT('Ctrl Pts',(3.99999756073998,2.30940248527475,-3.4333224880889));
#5537=CARTESIAN_POINT('Ctrl Pts',(3.99999852262203,2.3094025091568,-3.44798295458757));
#5538=CARTESIAN_POINT('Ctrl Pts',(4.00103676710518,2.31001134244407,-3.46258080581231));
#5539=CARTESIAN_POINT('Ctrl Pts',(4.00303436866837,2.31117707280252,-3.47695037704058));
#5540=CARTESIAN_POINT('Ctrl Pts',(4.00518415465818,2.31243161266605,-3.4924146735626));
#5541=CARTESIAN_POINT('Ctrl Pts',(4.00844429763966,2.31432976392346,-3.50761419176313));
#5542=CARTESIAN_POINT('Ctrl Pts',(4.01270080012744,2.31679499682455,-3.5224009318679));
#5543=CARTESIAN_POINT('Ctrl Pts',(4.01718844624318,2.3193941008741,-3.53799064595499));
#5544=CARTESIAN_POINT('Ctrl Pts',(4.0227826569856,2.32262219950312,-3.55312229806423));
#5545=CARTESIAN_POINT('Ctrl Pts',(4.02934571990586,2.32639953709204,-3.56768227773151));
#5546=CARTESIAN_POINT('Ctrl Pts',(4.03667602891417,2.330618459277,-3.58394437233773));
#5547=CARTESIAN_POINT('Ctrl Pts',(4.04521392823684,2.33552138396257,-3.5994949397553));
#5548=CARTESIAN_POINT('Ctrl Pts',(4.05477952071165,2.34103159972093,-3.61423009542096));
#5549=CARTESIAN_POINT('Ctrl Pts',(4.0575116841041,2.3426054499366,-3.61843881045851));
#5550=CARTESIAN_POINT('Ctrl Pts',(4.0603278059077,2.34422908860512,-3.6225812136314));
#5551=CARTESIAN_POINT('Ctrl Pts',(4.06322399022508,2.34590128842043,-3.62665524106974));
#5552=CARTESIAN_POINT('Ctrl Pts',(4.07427305149928,2.35228079890645,-3.64219782188164));
#5553=CARTESIAN_POINT('Ctrl Pts',(4.08643786251645,2.35931417813704,-3.65664956360123));
#5554=CARTESIAN_POINT('Ctrl Pts',(4.09949569192928,2.36685747216364,-3.66990623170327));
#5555=CARTESIAN_POINT('Ctrl Pts',(4.11717199569582,2.37706878312497,-3.68785170218656));
#5556=CARTESIAN_POINT('Ctrl Pts',(4.13648438951043,2.38821496403467,-3.70360921006995));
#5557=CARTESIAN_POINT('Ctrl Pts',(4.15691115197695,2.40000263229036,-3.7169911223592));
#5558=CARTESIAN_POINT('Ctrl Pts',(4.17428643035753,2.41002938115652,-3.72837395660282));
#5559=CARTESIAN_POINT('Ctrl Pts',(4.19247008634537,2.42052372384928,-3.73803875904013));
#5560=CARTESIAN_POINT('Ctrl Pts',(4.21114049304847,2.4313030972536,-3.74588525588109));
#5561=CARTESIAN_POINT('Ctrl Pts',(0.175002511812157,4.71983990082062,-3.46925408785825));
#5562=CARTESIAN_POINT('Ctrl Pts',(0.140404888673282,4.69986495378807,-3.68688706832704));
#5563=CARTESIAN_POINT('Ctrl Pts',(0.0244873395123948,4.87704277227473,-3.75116187409402));
#5564=CARTESIAN_POINT('Ctrl Pts',(-0.527628059414645,4.31417595138197,-3.32032231920172));
#5565=CARTESIAN_POINT('Ctrl Pts',(-0.546961429541692,4.30301382493627,-3.53526375354374));
#5566=CARTESIAN_POINT('Ctrl Pts',(-0.664094766059743,4.47107830999488,-3.60214640694596));
#5567=CARTESIAN_POINT('Ctrl Pts',(-1.24380216504891,3.90069263870738,-3.22314629010981));
#5568=CARTESIAN_POINT('Ctrl Pts',(-1.25717207227574,3.8929735191712,-3.43325269455078));
#5569=CARTESIAN_POINT('Ctrl Pts',(-1.36058516243547,4.06129624212829,-3.50505407716496));
#5570=CARTESIAN_POINT('Ctrl Pts',(-2.72574186843599,3.04509435203406,-3.22059942984405));
#5571=CARTESIAN_POINT('Ctrl Pts',(-2.71276256563901,3.05258795599751,-3.43061871662663));
#5572=CARTESIAN_POINT('Ctrl Pts',(-2.80708041617863,3.22596901922515,-3.50250721526044));
#5573=CARTESIAN_POINT('Ctrl Pts',(-3.45506866893449,2.62401732743904,-3.31662087526396));
#5574=CARTESIAN_POINT('Ctrl Pts',(-3.43631992298762,2.63484192096129,-3.53154229295572));
#5575=CARTESIAN_POINT('Ctrl Pts',(-3.52287509501967,2.82035290322543,-3.59844171492059));
#5576=CARTESIAN_POINT('Ctrl Pts',(-4.17564817396606,2.20799055623653,-3.46939095956406));
#5577=CARTESIAN_POINT('Ctrl Pts',(-4.14104229781062,2.22797026815042,-3.68702768697362));
#5578=CARTESIAN_POINT('Ctrl Pts',(-4.23652569453656,2.41695347538647,-3.75129874579984));
#5579=CARTESIAN_POINT('Ctrl Pts',(2.82335279537585E-12,4.86260619451211,
-3.7458852558811));
#5580=CARTESIAN_POINT('Ctrl Pts',(8.94255681535868E-9,4.83806530590424,
-3.73695337648466));
#5581=CARTESIAN_POINT('Ctrl Pts',(-2.9647450864845E-6,4.8143200797156,-3.72569031308144));
#5582=CARTESIAN_POINT('Ctrl Pts',(-7.79485668908126E-6,4.79186832593817,
-3.7122568151317));
#5583=CARTESIAN_POINT('Ctrl Pts',(-1.18956587044119E-5,4.77280661376393,
-3.70085167173177));
#5584=CARTESIAN_POINT('Ctrl Pts',(-1.50182025258554E-5,4.75467338932713,
-3.68788163056771));
#5585=CARTESIAN_POINT('Ctrl Pts',(-1.19717952318522E-5,4.73777305584639,
-3.67343984368836));
#5586=CARTESIAN_POINT('Ctrl Pts',(-9.24889085760412E-6,4.72266739612336,
-3.6605316535251));
#5587=CARTESIAN_POINT('Ctrl Pts',(-7.16403024165593E-7,4.70854584288659,
-3.64644578532448));
#5588=CARTESIAN_POINT('Ctrl Pts',(1.49498629956454E-6,4.69565301047662,
-3.63126295026017));
#5589=CARTESIAN_POINT('Ctrl Pts',(1.71734419142002E-6,4.69435662046335,
-3.62973629768884));
#5590=CARTESIAN_POINT('Ctrl Pts',(1.85602259680142E-6,4.69307268216863,
-3.62819858241928));
#5591=CARTESIAN_POINT('Ctrl Pts',(1.88466842695255E-6,4.69180146380839,
-3.62664990860529));
#5592=CARTESIAN_POINT('Ctrl Pts',(2.13950640372796E-6,4.680492497957,-3.61287265378804));
#5593=CARTESIAN_POINT('Ctrl Pts',(-1.9306210438466E-5,4.67025176882188,
-3.59831217982513));
#5594=CARTESIAN_POINT('Ctrl Pts',(-3.48040781505873E-5,4.66124444713254,
-3.58305396405286));
#5595=CARTESIAN_POINT('Ctrl Pts',(-4.91300462124437E-5,4.652918230569,-3.56894952621052));
#5596=CARTESIAN_POINT('Ctrl Pts',(-5.84590505708E-5,4.64564664360582,-3.55424735099498));
#5597=CARTESIAN_POINT('Ctrl Pts',(-5.74159969723896E-5,4.63958221831933,
-3.53904369510472));
#5598=CARTESIAN_POINT('Ctrl Pts',(-5.64316965346851E-5,4.63385939019907,
-3.52469643129172));
#5599=CARTESIAN_POINT('Ctrl Pts',(-4.66685024715262E-5,4.62921266308804,
-3.50990174309249));
#5600=CARTESIAN_POINT('Ctrl Pts',(-3.48265015805382E-5,4.62577768814575,
-3.49478366353225));
#5601=CARTESIAN_POINT('Ctrl Pts',(-2.3677727972645E-5,4.62254379563611,
-3.48055059194621));
#5602=CARTESIAN_POINT('Ctrl Pts',(-1.13157927300613E-5,4.6203850753921,
-3.46603083046657));
#5603=CARTESIAN_POINT('Ctrl Pts',(-5.72057276286163E-6,4.61940554316572,
-3.45137322816867));
#5604=CARTESIAN_POINT('Ctrl Pts',(-3.43072437850262E-6,4.61900466879454,
-3.4453745923443));
#5605=CARTESIAN_POINT('Ctrl Pts',(-2.25005174120207E-6,4.61880108620347,
-3.43935342011916));
#5606=CARTESIAN_POINT('Ctrl Pts',(-2.4394502271739E-6,4.61880074529695,
-3.43332218943429));
#5607=CARTESIAN_POINT('Ctrl Pts',(4.17500251181215,2.20836332945489,-3.46925408785824));
#5608=CARTESIAN_POINT('Ctrl Pts',(4.14040488867328,2.22833827648744,-3.68688706832703));
#5609=CARTESIAN_POINT('Ctrl Pts',(4.23588660588939,2.41731472804853,-3.75116187409402));
#5610=CARTESIAN_POINT('Ctrl Pts',(3.47237194058599,2.61402727889318,-3.32032231920177));
#5611=CARTESIAN_POINT('Ctrl Pts',(3.45303857046027,2.62518940534083,-3.53526375354359));
#5612=CARTESIAN_POINT('Ctrl Pts',(3.5400200157356,2.81066209292438,-3.60214640694587));
#5613=CARTESIAN_POINT('Ctrl Pts',(2.75619783495023,3.02751059156863,-3.22314629010981));
#5614=CARTESIAN_POINT('Ctrl Pts',(2.74282792772345,3.03522971110461,-3.43325269455059));
#5615=CARTESIAN_POINT('Ctrl Pts',(2.83689313675868,3.20894943574584,-3.50505407716491));
#5616=CARTESIAN_POINT('Ctrl Pts',(1.27425813156487,3.88310887824096,-3.22059942984405));
#5617=CARTESIAN_POINT('Ctrl Pts',(1.28723743436204,3.87561527427756,-3.43061871662681));
#5618=CARTESIAN_POINT('Ctrl Pts',(1.39023091438219,4.04398746048866,-3.50250721526049));
#5619=CARTESIAN_POINT('Ctrl Pts',(0.544931331064781,4.3041859028369,-3.31662087526338));
#5620=CARTESIAN_POINT('Ctrl Pts',(0.563680077013038,4.29336130931717,-3.5315422929541));
#5621=CARTESIAN_POINT('Ctrl Pts',(0.681059714319705,4.46107577825929,-3.5984417149206));
#5622=CARTESIAN_POINT('Ctrl Pts',(-0.175648173966052,4.72021267403898,-3.46939095956407));
#5623=CARTESIAN_POINT('Ctrl Pts',(-0.141042297810612,4.70023296212509,-3.68702768697363));
#5624=CARTESIAN_POINT('Ctrl Pts',(-0.0251197378185046,4.87741561294741,
-3.75129874579984));
#5625=CARTESIAN_POINT('',(0.,0.,0.));
#5626=CARTESIAN_POINT('',(0.,0.,0.));
#5627=CARTESIAN_POINT('',(0.,0.,0.));
#5628=CARTESIAN_POINT('',(0.,0.,0.));
#5629=CARTESIAN_POINT('',(0.,0.,123.));
#5630=CARTESIAN_POINT('',(53.3333333333333,-15.,162.5));
#5631=CARTESIAN_POINT('',(53.3333333333333,-35.,162.5));
#5632=CARTESIAN_POINT('',(0.,0.,-123.));
#5633=CARTESIAN_POINT('',(136.666666666667,-15.,162.5));
#5634=CARTESIAN_POINT('',(220.,-15.,162.5));
#5635=CARTESIAN_POINT('',(303.333333333333,-15.,162.5));
#5636=CARTESIAN_POINT('',(386.666666666667,-15.,162.5));
#5637=CARTESIAN_POINT('',(136.666666666667,-35.,162.5));
#5638=CARTESIAN_POINT('',(220.,-35.,162.5));
#5639=CARTESIAN_POINT('',(303.333333333333,-35.,162.5));
#5640=CARTESIAN_POINT('',(386.666666666667,-35.,162.5));
#5641=CARTESIAN_POINT('',(440.,0.,0.));
#5642=CARTESIAN_POINT('',(88.,0.,-123.));
#5643=CARTESIAN_POINT('',(176.,0.,-123.));
#5644=CARTESIAN_POINT('',(264.,0.,-123.));
#5645=CARTESIAN_POINT('',(352.,0.,-123.));
#5646=CARTESIAN_POINT('',(440.,0.,-123.));
#5647=CARTESIAN_POINT('',(88.,0.,0.));
#5648=CARTESIAN_POINT('',(176.,0.,0.));
#5649=CARTESIAN_POINT('',(264.,0.,0.));
#5650=CARTESIAN_POINT('',(352.,0.,0.));
#5651=CARTESIAN_POINT('',(440.,0.,0.));
#5652=CARTESIAN_POINT('',(88.,0.,123.));
#5653=CARTESIAN_POINT('',(176.,0.,123.));
#5654=CARTESIAN_POINT('',(264.,0.,123.));
#5655=CARTESIAN_POINT('',(352.,0.,123.));
#5656=CARTESIAN_POINT('',(440.,0.,123.));
#5657=CARTESIAN_POINT('',(88.,0.,0.));
#5658=CARTESIAN_POINT('',(176.,0.,0.));
#5659=CARTESIAN_POINT('',(264.,0.,0.));
#5660=CARTESIAN_POINT('',(352.,0.,0.));
#5661=CARTESIAN_POINT('',(440.,0.,0.));
#5662=CARTESIAN_POINT('',(53.3333333333333,-35.,-162.5));
#5663=CARTESIAN_POINT('',(136.666666666667,-35.,-162.5));
#5664=CARTESIAN_POINT('',(220.,-15.,-162.5));
#5665=CARTESIAN_POINT('',(220.,-35.,-162.5));
#5666=CARTESIAN_POINT('',(53.3333333333333,-15.,-162.5));
#5667=CARTESIAN_POINT('',(136.666666666667,-15.,-162.5));
#5668=CARTESIAN_POINT('',(386.666666666667,-15.,-162.5));
#5669=CARTESIAN_POINT('',(303.333333333333,-15.,-162.5));
#5670=CARTESIAN_POINT('',(386.666666666667,-35.,-162.5));
#5671=CARTESIAN_POINT('',(303.333333333333,-35.,-162.5));
#5672=UNCERTAINTY_MEASURE_WITH_UNIT(LENGTH_MEASURE(0.01),#5690,
'DISTANCE_ACCURACY_VALUE',
'Maximum model space distance between geometric entities at asserted c
onnectivities');
#5673=UNCERTAINTY_MEASURE_WITH_UNIT(LENGTH_MEASURE(0.01),#5690,
'DISTANCE_ACCURACY_VALUE',
'Maximum model space distance between geometric entities at asserted c
onnectivities');
#5674=UNCERTAINTY_MEASURE_WITH_UNIT(LENGTH_MEASURE(0.01),#5690,
'DISTANCE_ACCURACY_VALUE',
'Maximum model space distance between geometric entities at asserted c
onnectivities');
#5675=UNCERTAINTY_MEASURE_WITH_UNIT(LENGTH_MEASURE(0.01),#5690,
'DISTANCE_ACCURACY_VALUE',
'Maximum model space distance between geometric entities at asserted c
onnectivities');
#5676=UNCERTAINTY_MEASURE_WITH_UNIT(LENGTH_MEASURE(0.01),#5690,
'DISTANCE_ACCURACY_VALUE',
'Maximum model space distance between geometric entities at asserted c
onnectivities');
#5677=UNCERTAINTY_MEASURE_WITH_UNIT(LENGTH_MEASURE(0.01),#5690,
'DISTANCE_ACCURACY_VALUE',
'Maximum model space distance between geometric entities at asserted c
onnectivities');
#5678=UNCERTAINTY_MEASURE_WITH_UNIT(LENGTH_MEASURE(0.01),#5690,
'DISTANCE_ACCURACY_VALUE',
'Maximum model space distance between geometric entities at asserted c
onnectivities');
#5679=UNCERTAINTY_MEASURE_WITH_UNIT(LENGTH_MEASURE(0.01),#5690,
'DISTANCE_ACCURACY_VALUE',
'Maximum model space distance between geometric entities at asserted c
onnectivities');
#5680=UNCERTAINTY_MEASURE_WITH_UNIT(LENGTH_MEASURE(0.01),#5690,
'DISTANCE_ACCURACY_VALUE',
'Maximum model space distance between geometric entities at asserted c
onnectivities');
#5681=(
GEOMETRIC_REPRESENTATION_CONTEXT(3)
GLOBAL_UNCERTAINTY_ASSIGNED_CONTEXT((#5672))
GLOBAL_UNIT_ASSIGNED_CONTEXT((#5690,#5692,#5693))
REPRESENTATION_CONTEXT('','3D')
);
#5682=(
GEOMETRIC_REPRESENTATION_CONTEXT(3)
GLOBAL_UNCERTAINTY_ASSIGNED_CONTEXT((#5673))
GLOBAL_UNIT_ASSIGNED_CONTEXT((#5690,#5692,#5693))
REPRESENTATION_CONTEXT('','3D')
);
#5683=(
GEOMETRIC_REPRESENTATION_CONTEXT(3)
GLOBAL_UNCERTAINTY_ASSIGNED_CONTEXT((#5674))
GLOBAL_UNIT_ASSIGNED_CONTEXT((#5690,#5692,#5693))
REPRESENTATION_CONTEXT('','3D')
);
#5684=(
GEOMETRIC_REPRESENTATION_CONTEXT(3)
GLOBAL_UNCERTAINTY_ASSIGNED_CONTEXT((#5675))
GLOBAL_UNIT_ASSIGNED_CONTEXT((#5690,#5692,#5693))
REPRESENTATION_CONTEXT('','3D')
);
#5685=(
GEOMETRIC_REPRESENTATION_CONTEXT(3)
GLOBAL_UNCERTAINTY_ASSIGNED_CONTEXT((#5676))
GLOBAL_UNIT_ASSIGNED_CONTEXT((#5690,#5692,#5693))
REPRESENTATION_CONTEXT('','3D')
);
#5686=(
GEOMETRIC_REPRESENTATION_CONTEXT(3)
GLOBAL_UNCERTAINTY_ASSIGNED_CONTEXT((#5677))
GLOBAL_UNIT_ASSIGNED_CONTEXT((#5690,#5692,#5693))
REPRESENTATION_CONTEXT('','3D')
);
#5687=(
GEOMETRIC_REPRESENTATION_CONTEXT(3)
GLOBAL_UNCERTAINTY_ASSIGNED_CONTEXT((#5678))
GLOBAL_UNIT_ASSIGNED_CONTEXT((#5690,#5692,#5693))
REPRESENTATION_CONTEXT('','3D')
);
#5688=(
GEOMETRIC_REPRESENTATION_CONTEXT(3)
GLOBAL_UNCERTAINTY_ASSIGNED_CONTEXT((#5679))
GLOBAL_UNIT_ASSIGNED_CONTEXT((#5690,#5692,#5693))
REPRESENTATION_CONTEXT('','3D')
);
#5689=(
GEOMETRIC_REPRESENTATION_CONTEXT(3)
GLOBAL_UNCERTAINTY_ASSIGNED_CONTEXT((#5680))
GLOBAL_UNIT_ASSIGNED_CONTEXT((#5690,#5692,#5693))
REPRESENTATION_CONTEXT('','3D')
);
#5690=(
LENGTH_UNIT()
NAMED_UNIT(*)
SI_UNIT(.MILLI.,.METRE.)
);
#5691=(
LENGTH_UNIT()
NAMED_UNIT(*)
SI_UNIT($,.METRE.)
);
#5692=(
NAMED_UNIT(*)
PLANE_ANGLE_UNIT()
SI_UNIT($,.RADIAN.)
);
#5693=(
NAMED_UNIT(*)
SI_UNIT($,.STERADIAN.)
SOLID_ANGLE_UNIT()
);
#5694=SHAPE_DEFINITION_REPRESENTATION(#5702,#5757);
#5695=SHAPE_DEFINITION_REPRESENTATION(#5703,#5758);
#5696=SHAPE_DEFINITION_REPRESENTATION(#5704,#5759);
#5697=SHAPE_DEFINITION_REPRESENTATION(#5705,#5760);
#5698=SHAPE_DEFINITION_REPRESENTATION(#5706,#5761);
#5699=SHAPE_DEFINITION_REPRESENTATION(#5707,#5762);
#5700=SHAPE_DEFINITION_REPRESENTATION(#5708,#5763);
#5701=SHAPE_DEFINITION_REPRESENTATION(#5709,#5764);
#5702=PRODUCT_DEFINITION_SHAPE('',$,#5766);
#5703=PRODUCT_DEFINITION_SHAPE('',$,#5767);
#5704=PRODUCT_DEFINITION_SHAPE('',$,#5768);
#5705=PRODUCT_DEFINITION_SHAPE('',$,#5769);
#5706=PRODUCT_DEFINITION_SHAPE('',$,#5770);
#5707=PRODUCT_DEFINITION_SHAPE('',$,#5771);
#5708=PRODUCT_DEFINITION_SHAPE('',$,#5772);
#5709=PRODUCT_DEFINITION_SHAPE('',$,#5773);
#5710=PRODUCT_DEFINITION_SHAPE($,$,#152);
#5711=PRODUCT_DEFINITION_SHAPE($,$,#153);
#5712=PRODUCT_DEFINITION_SHAPE($,$,#154);
#5713=PRODUCT_DEFINITION_SHAPE($,$,#155);
#5714=PRODUCT_DEFINITION_SHAPE($,$,#156);
#5715=PRODUCT_DEFINITION_SHAPE($,$,#157);
#5716=PRODUCT_DEFINITION_SHAPE($,$,#158);
#5717=PRODUCT_DEFINITION_SHAPE($,$,#159);
#5718=PRODUCT_DEFINITION_SHAPE($,$,#160);
#5719=PRODUCT_DEFINITION_SHAPE($,$,#161);
#5720=PRODUCT_DEFINITION_SHAPE($,$,#162);
#5721=PRODUCT_DEFINITION_SHAPE($,$,#163);
#5722=PRODUCT_DEFINITION_SHAPE($,$,#164);
#5723=PRODUCT_DEFINITION_SHAPE($,$,#165);
#5724=PRODUCT_DEFINITION_SHAPE($,$,#166);
#5725=PRODUCT_DEFINITION_SHAPE($,$,#167);
#5726=PRODUCT_DEFINITION_SHAPE($,$,#168);
#5727=PRODUCT_DEFINITION_SHAPE($,$,#169);
#5728=PRODUCT_DEFINITION_SHAPE($,$,#170);
#5729=PRODUCT_DEFINITION_SHAPE($,$,#171);
#5730=PRODUCT_DEFINITION_SHAPE($,$,#172);
#5731=PRODUCT_DEFINITION_SHAPE($,$,#173);
#5732=PRODUCT_DEFINITION_SHAPE($,$,#174);
#5733=PRODUCT_DEFINITION_SHAPE($,$,#175);
#5734=PRODUCT_DEFINITION_SHAPE($,$,#176);
#5735=PRODUCT_DEFINITION_SHAPE($,$,#177);
#5736=PRODUCT_DEFINITION_SHAPE($,$,#178);
#5737=PRODUCT_DEFINITION_SHAPE($,$,#179);
#5738=PRODUCT_DEFINITION_SHAPE($,$,#180);
#5739=PRODUCT_DEFINITION_SHAPE($,$,#181);
#5740=PRODUCT_DEFINITION_SHAPE($,$,#182);
#5741=PRODUCT_DEFINITION_SHAPE($,$,#183);
#5742=PRODUCT_DEFINITION_SHAPE($,$,#184);
#5743=PRODUCT_DEFINITION_SHAPE($,$,#185);
#5744=PRODUCT_DEFINITION_SHAPE($,$,#186);
#5745=PRODUCT_DEFINITION_SHAPE($,$,#187);
#5746=PRODUCT_DEFINITION_SHAPE($,$,#188);
#5747=PRODUCT_DEFINITION_SHAPE($,$,#189);
#5748=PRODUCT_DEFINITION_SHAPE($,$,#190);
#5749=PRODUCT_DEFINITION_SHAPE($,$,#191);
#5750=PRODUCT_DEFINITION_SHAPE($,$,#192);
#5751=PRODUCT_DEFINITION_SHAPE($,$,#193);
#5752=PRODUCT_DEFINITION_SHAPE($,$,#194);
#5753=PRODUCT_DEFINITION_SHAPE($,$,#195);
#5754=PRODUCT_DEFINITION_SHAPE($,$,#196);
#5755=PRODUCT_DEFINITION_SHAPE($,$,#197);
#5756=PRODUCT_DEFINITION_SHAPE($,$,#198);
#5757=SHAPE_REPRESENTATION('',(#3046,#3322,#3323,#3324,#3325,#3326,#3327,
#3328,#3329,#3330,#3331,#3332,#3333,#3334,#3335,#3336,#3337,#3338,#3339,
#3340,#3341,#3342,#3343,#3344,#3345,#3346,#3347,#3348,#3349,#3350,#3351,
#3352,#3353,#3354,#3355,#3356,#3357,#3358,#3359,#3360,#3361,#3362,#3363,
#3364,#3365,#3366,#3367,#3368),#5681);
#5758=SHAPE_REPRESENTATION('',(#3047),#5682);
#5759=SHAPE_REPRESENTATION('',(#3108),#5683);
#5760=SHAPE_REPRESENTATION('',(#3156),#5684);
#5761=SHAPE_REPRESENTATION('',(#3186),#5685);
#5762=SHAPE_REPRESENTATION('',(#3229),#5686);
#5763=SHAPE_REPRESENTATION('',(#3246),#5687);
#5764=SHAPE_REPRESENTATION('',(#3284),#5688);
#5765=PRODUCT_DEFINITION_CONTEXT('part definition',#5791,'design');
#5766=PRODUCT_DEFINITION('Conveyor Roller Module',
'MAS-187',#5774,#5765);
#5767=PRODUCT_DEFINITION('base table','base table',#5775,#5765);
#5768=PRODUCT_DEFINITION('side rail','side rail',#5776,#5765);
#5769=PRODUCT_DEFINITION('roller axis','roller axis',#5777,#5765);
#5770=PRODUCT_DEFINITION(
'angular contact ball bearing_68_iso_ISO 15 ABB - 1720 - 28,SI,NC,28_6
8',
'angular contact ball bearing_68_iso_ISO 15 ABB - 1720 - 28,SI,NC,28_6
8',#5778,#5765);
#5771=PRODUCT_DEFINITION('roller','roller',#5779,#5765);
#5772=PRODUCT_DEFINITION(
'socket head cap screw_iso_ISO 4762 M5 x 20 - 20N',
'socket head cap screw_iso_ISO 4762 M5 x 20 - 20N',#5780,#5765);
#5773=PRODUCT_DEFINITION(
'hex flange nut gradea_iso_ISO - 4161 - M5 - N',
'hex flange nut gradea_iso_ISO - 4161 - M5 - N',#5781,#5765);
#5774=PRODUCT_DEFINITION_FORMATION('',$,#5793);
#5775=PRODUCT_DEFINITION_FORMATION('',$,#5794);
#5776=PRODUCT_DEFINITION_FORMATION('',$,#5795);
#5777=PRODUCT_DEFINITION_FORMATION('',$,#5796);
#5778=PRODUCT_DEFINITION_FORMATION('',$,#5797);
#5779=PRODUCT_DEFINITION_FORMATION('',$,#5798);
#5780=PRODUCT_DEFINITION_FORMATION('',$,#5799);
#5781=PRODUCT_DEFINITION_FORMATION('',$,#5800);
#5782=PRODUCT_RELATED_PRODUCT_CATEGORY(
'MAS-187',
'MAS-187',(#5793));
#5783=PRODUCT_RELATED_PRODUCT_CATEGORY('base table','base table',(#5794));
#5784=PRODUCT_RELATED_PRODUCT_CATEGORY('side rail','side rail',(#5795));
#5785=PRODUCT_RELATED_PRODUCT_CATEGORY('roller axis','roller axis',(#5796));
#5786=PRODUCT_RELATED_PRODUCT_CATEGORY(
'angular contact ball bearing_68_iso_ISO 15 ABB - 1720 - 28,SI,NC,28_6
8',
'angular contact ball bearing_68_iso_ISO 15 ABB - 1720 - 28,SI,NC,28_6
8',(#5797));
#5787=PRODUCT_RELATED_PRODUCT_CATEGORY('roller','roller',(#5798));
#5788=PRODUCT_RELATED_PRODUCT_CATEGORY(
'socket head cap screw_iso_ISO 4762 M5 x 20 - 20N',
'socket head cap screw_iso_ISO 4762 M5 x 20 - 20N',(#5799));
#5789=PRODUCT_RELATED_PRODUCT_CATEGORY(
'hex flange nut gradea_iso_ISO - 4161 - M5 - N',
'hex flange nut gradea_iso_ISO - 4161 - M5 - N',(#5800));
#5790=APPLICATION_PROTOCOL_DEFINITION('international standard',
'automotive_design',2009,#5791);
#5791=APPLICATION_CONTEXT(
'Core Data for Automotive Mechanical Design Process');
#5792=PRODUCT_CONTEXT('part definition',#5791,'mechanical');
#5793=PRODUCT('Conveyor Roller Module',
'MAS-187','STEP AP214',(#5792));
#5794=PRODUCT('base table','base table',$,(#5792));
#5795=PRODUCT('side rail','side rail',$,(#5792));
#5796=PRODUCT('roller axis','roller axis',$,(#5792));
#5797=PRODUCT(
'angular contact ball bearing_68_iso_ISO 15 ABB - 1720 - 28,SI,NC,28_6
8',
'angular contact ball bearing_68_iso_ISO 15 ABB - 1720 - 28,SI,NC,28_6
8',$,(#5792));
#5798=PRODUCT('roller','roller',$,(#5792));
#5799=PRODUCT('socket head cap screw_iso_ISO 4762 M5 x 20 - 20N',
'socket head cap screw_iso_ISO 4762 M5 x 20 - 20N',$,(#5792));
#5800=PRODUCT('hex flange nut gradea_iso_ISO - 4161 - M5 - N',
'hex flange nut gradea_iso_ISO - 4161 - M5 - N',$,(#5792));
#5801=PRESENTATION_STYLE_ASSIGNMENT((#5807));
#5802=PRESENTATION_STYLE_ASSIGNMENT((#5808));
#5803=PRESENTATION_STYLE_ASSIGNMENT((#5809));
#5804=PRESENTATION_STYLE_ASSIGNMENT((#5810));
#5805=PRESENTATION_STYLE_ASSIGNMENT((#5811));
#5806=PRESENTATION_STYLE_ASSIGNMENT((#5812));
#5807=SURFACE_STYLE_USAGE(.BOTH.,#5813);
#5808=SURFACE_STYLE_USAGE(.BOTH.,#5814);
#5809=SURFACE_STYLE_USAGE(.BOTH.,#5815);
#5810=SURFACE_STYLE_USAGE(.BOTH.,#5816);
#5811=SURFACE_STYLE_USAGE(.BOTH.,#5817);
#5812=SURFACE_STYLE_USAGE(.BOTH.,#5818);
#5813=SURFACE_SIDE_STYLE('',(#5819));
#5814=SURFACE_SIDE_STYLE('',(#5820));
#5815=SURFACE_SIDE_STYLE('',(#5821));
#5816=SURFACE_SIDE_STYLE('',(#5822));
#5817=SURFACE_SIDE_STYLE('',(#5823));
#5818=SURFACE_SIDE_STYLE('',(#5824));
#5819=SURFACE_STYLE_FILL_AREA(#5825);
#5820=SURFACE_STYLE_FILL_AREA(#5826);
#5821=SURFACE_STYLE_FILL_AREA(#5827);
#5822=SURFACE_STYLE_FILL_AREA(#5828);
#5823=SURFACE_STYLE_FILL_AREA(#5829);
#5824=SURFACE_STYLE_FILL_AREA(#5830);
#5825=FILL_AREA_STYLE('Steel - Satin',(#5831));
#5826=FILL_AREA_STYLE('Opaque(20,51,87)',(#5832));
#5827=FILL_AREA_STYLE('Opaque(97,158,199)',(#5833));
#5828=FILL_AREA_STYLE('Opaque(61,176,222)',(#5834));
#5829=FILL_AREA_STYLE('Opaque(122,133,145)',(#5835));
#5830=FILL_AREA_STYLE('Opaque(31,36,43)',(#5836));
#5831=FILL_AREA_STYLE_COLOUR('Steel - Satin',#5837);
#5832=FILL_AREA_STYLE_COLOUR('Opaque(20,51,87)',#5838);
#5833=FILL_AREA_STYLE_COLOUR('Opaque(97,158,199)',#5839);
#5834=FILL_AREA_STYLE_COLOUR('Opaque(61,176,222)',#5840);
#5835=FILL_AREA_STYLE_COLOUR('Opaque(122,133,145)',#5841);
#5836=FILL_AREA_STYLE_COLOUR('Opaque(31,36,43)',#5842);
#5837=COLOUR_RGB('Steel - Satin',0.627450980392157,0.627450980392157,0.627450980392157);
#5838=COLOUR_RGB('Opaque(20,51,87)',0.0784313725490196,0.2,0.341176470588235);
#5839=COLOUR_RGB('Opaque(97,158,199)',0.380392156862745,0.619607843137255,
0.780392156862745);
#5840=COLOUR_RGB('Opaque(61,176,222)',0.23921568627451,0.690196078431373,
0.870588235294118);
#5841=COLOUR_RGB('Opaque(122,133,145)',0.47843137254902,0.52156862745098,
0.568627450980392);
#5842=COLOUR_RGB('Opaque(31,36,43)',0.12156862745098,0.141176470588235,
0.168627450980392);
ENDSEC;
END-ISO-10303-21;
